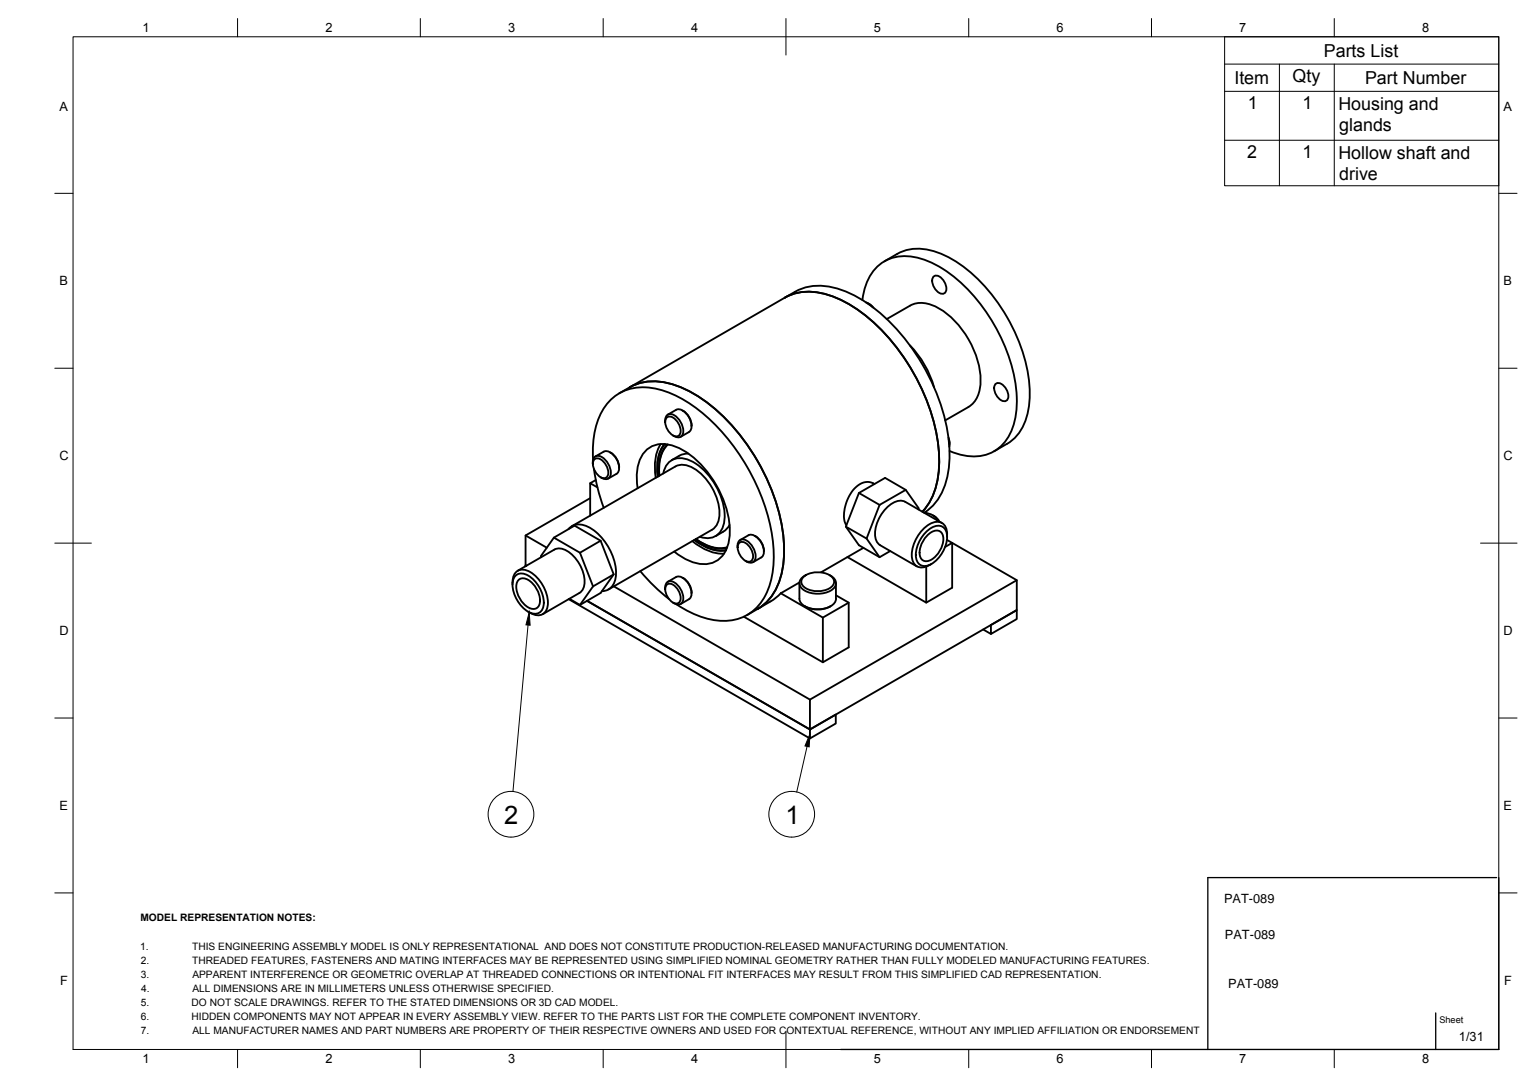
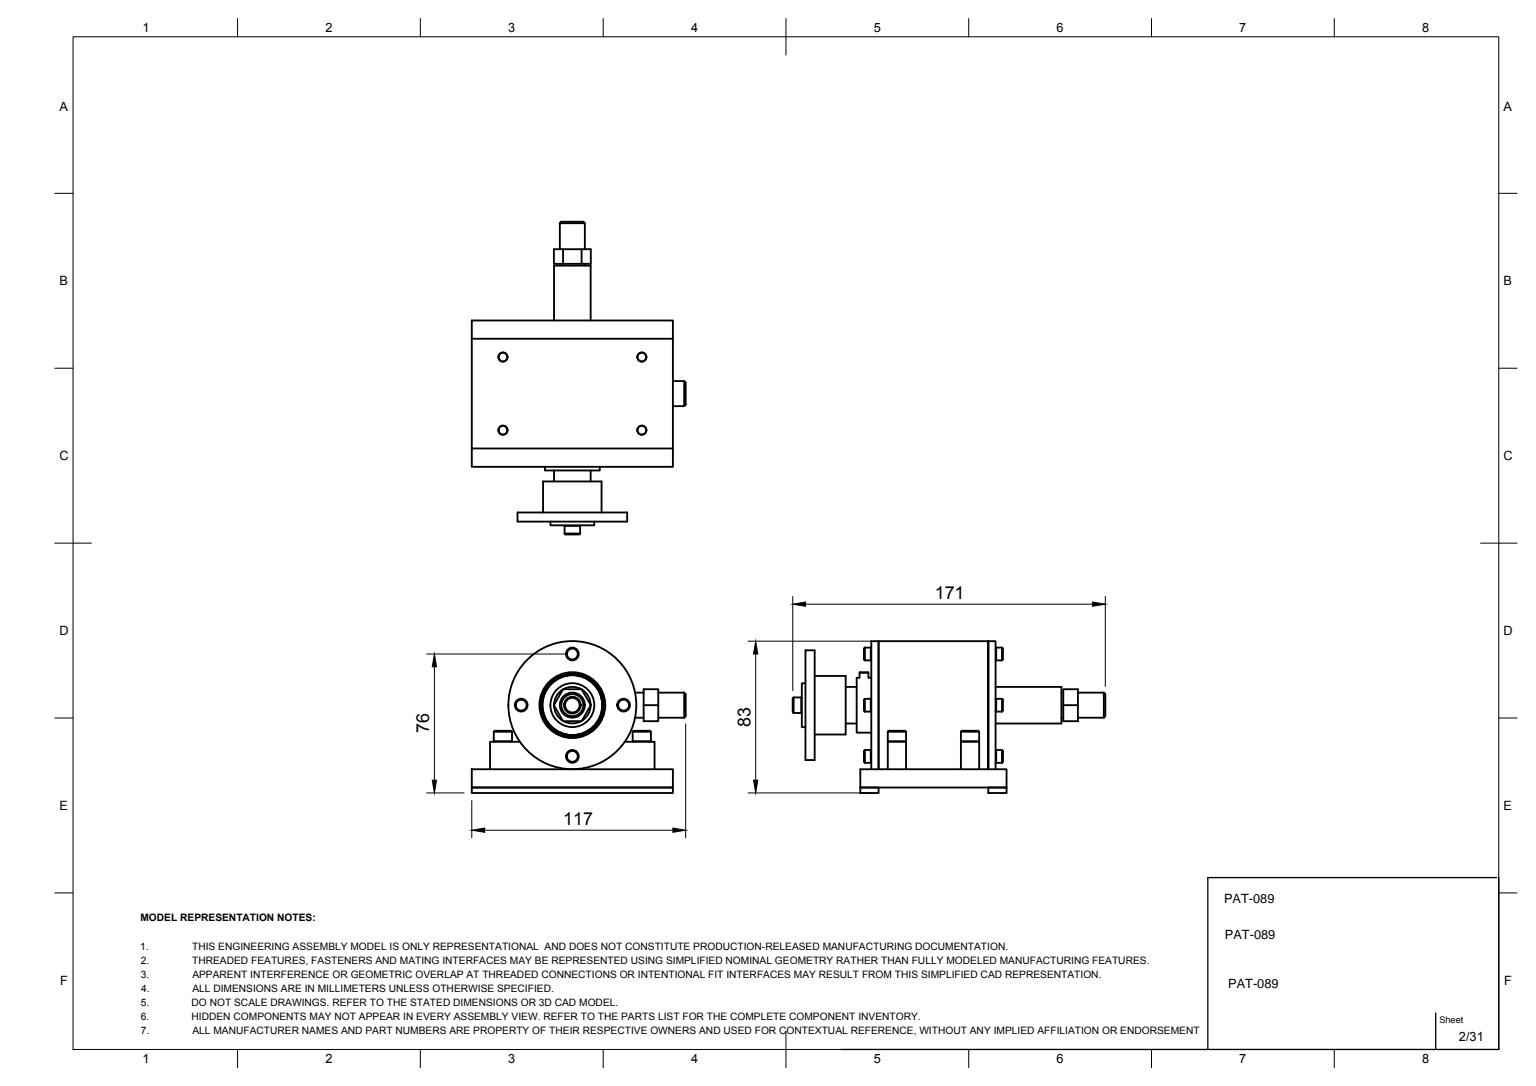
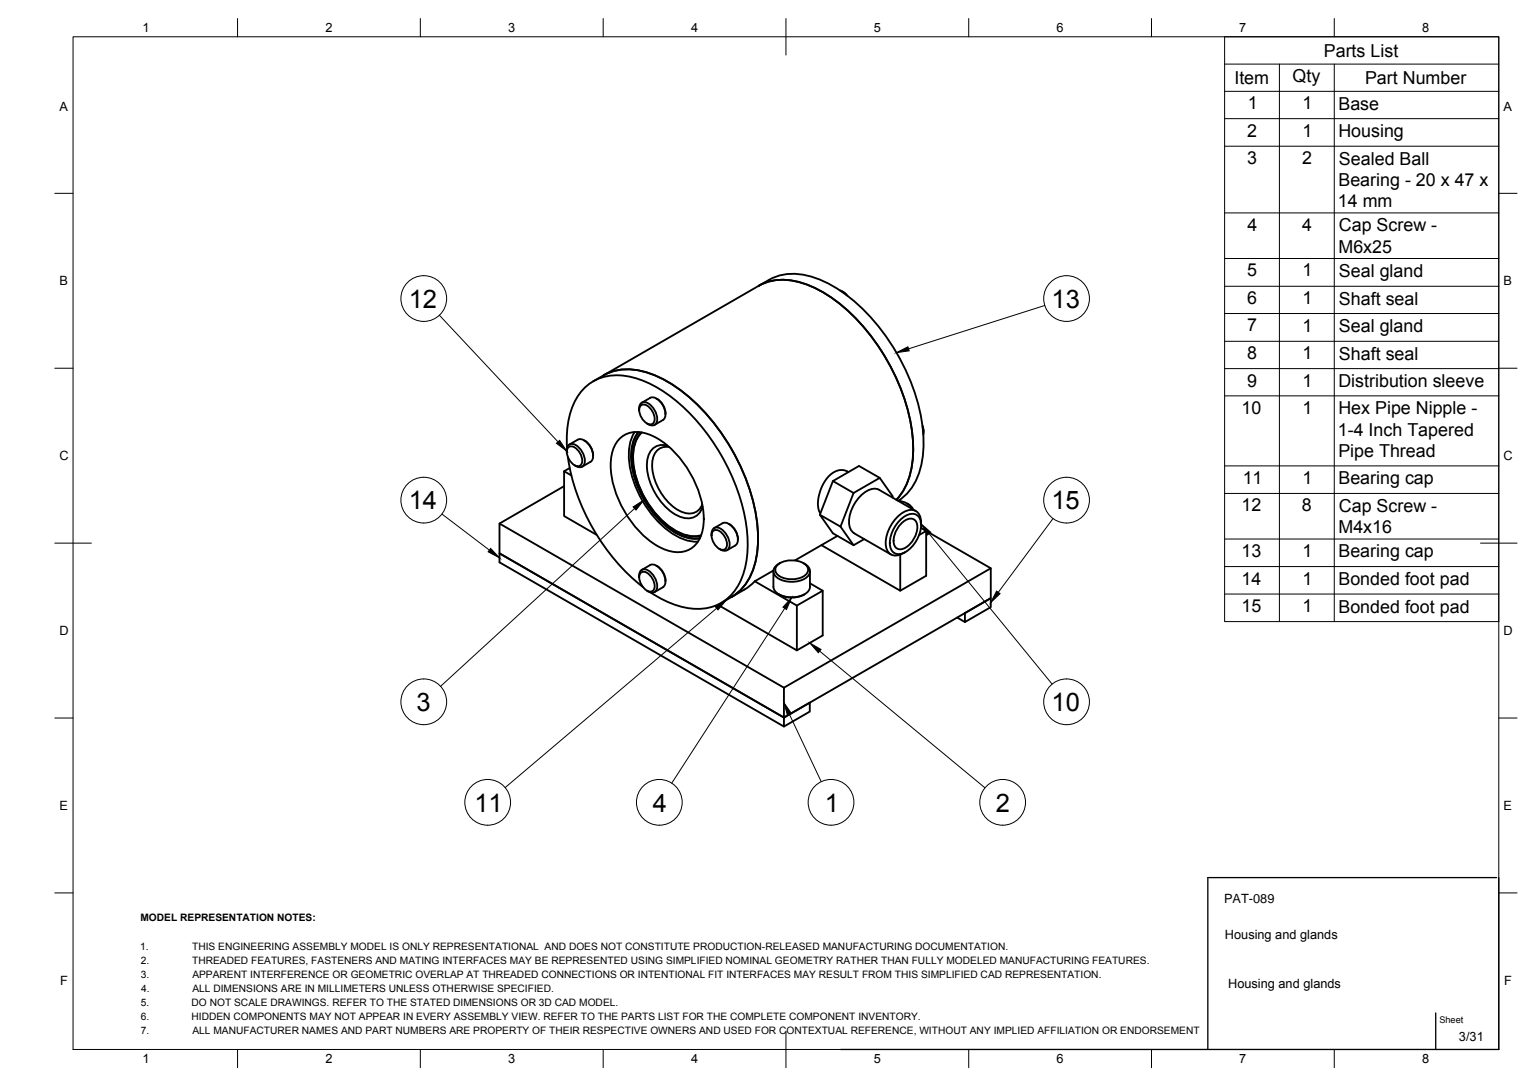
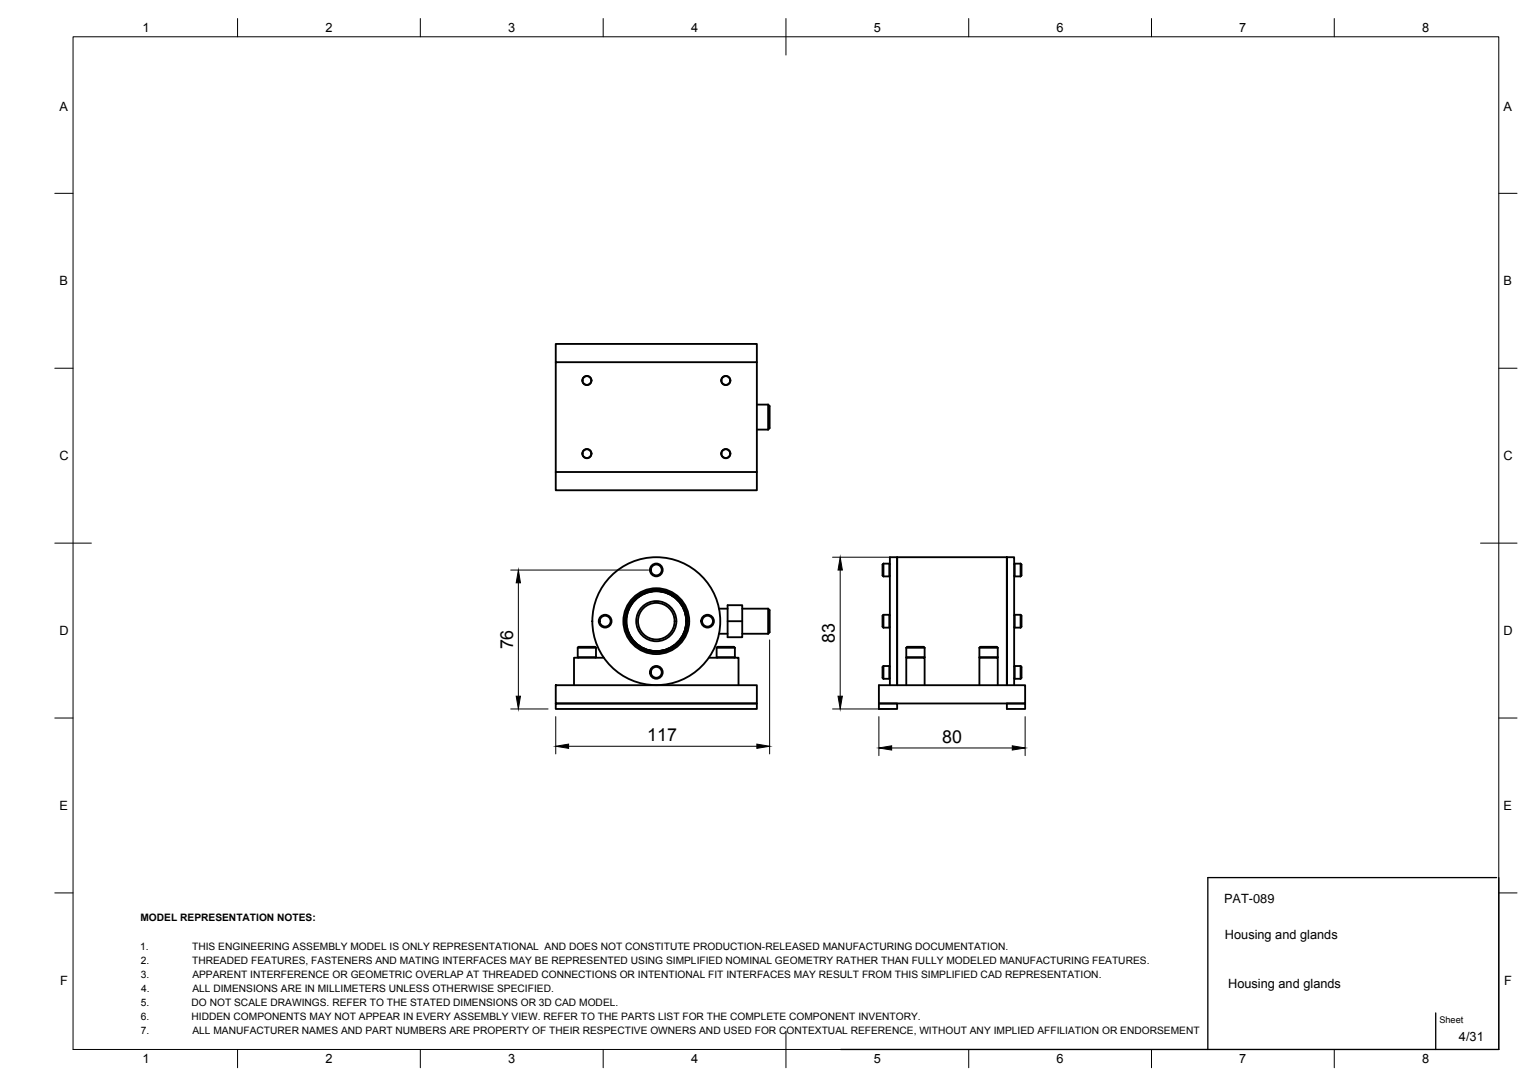
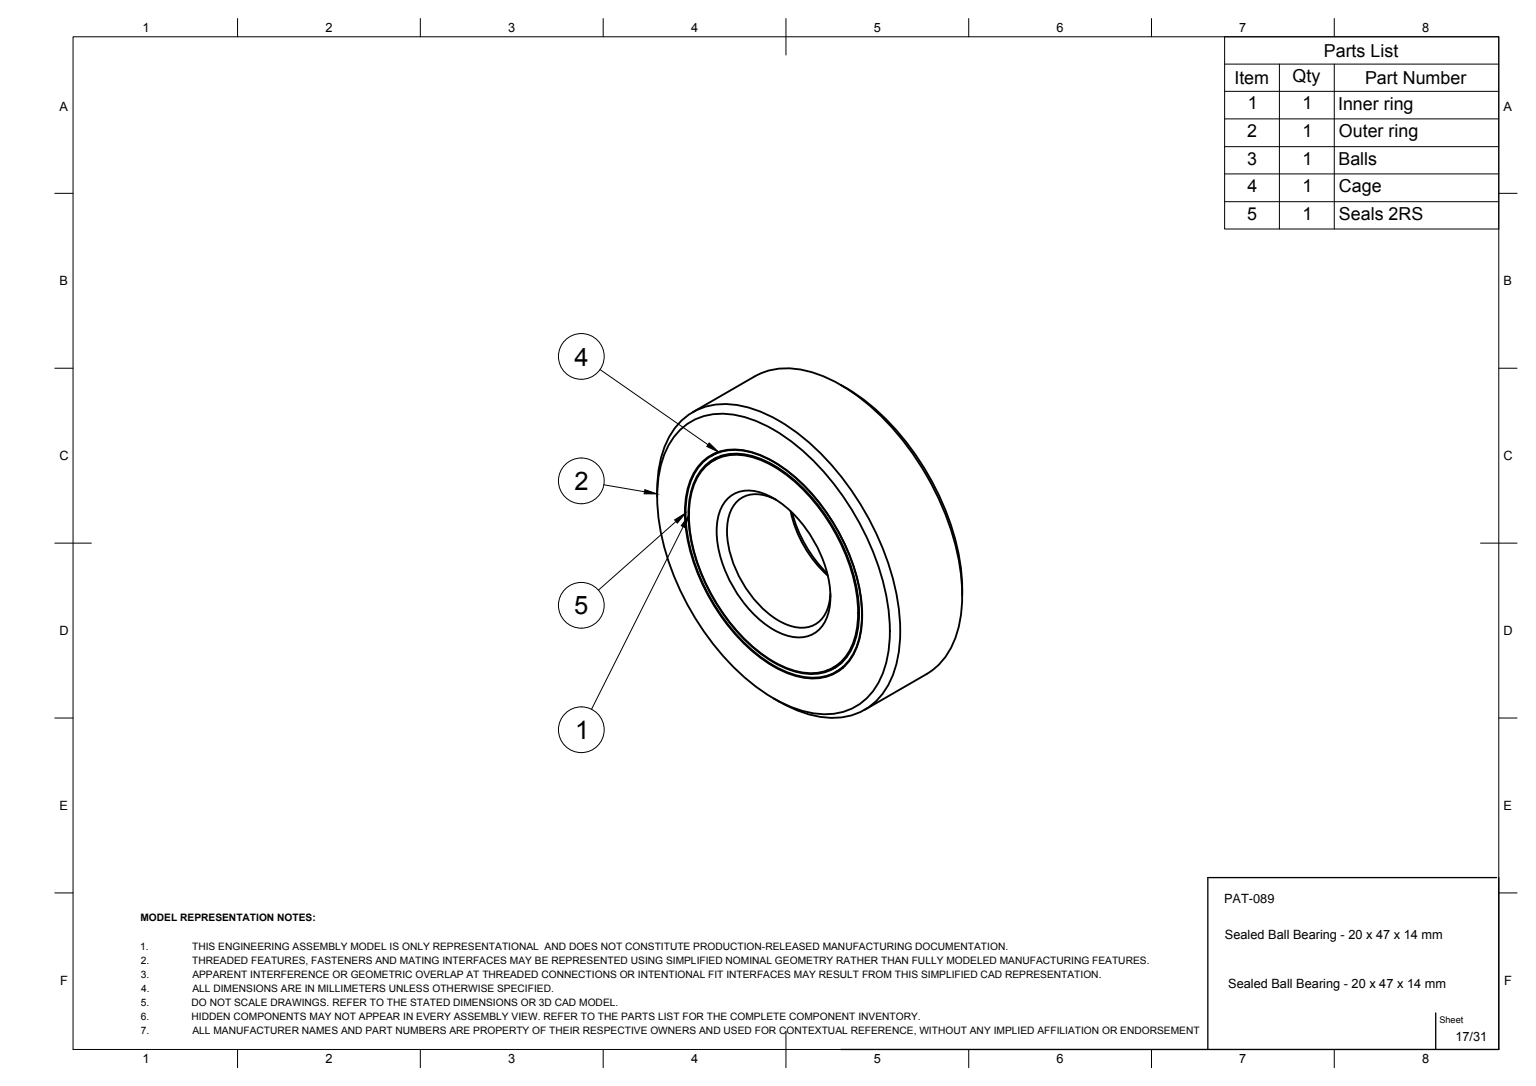
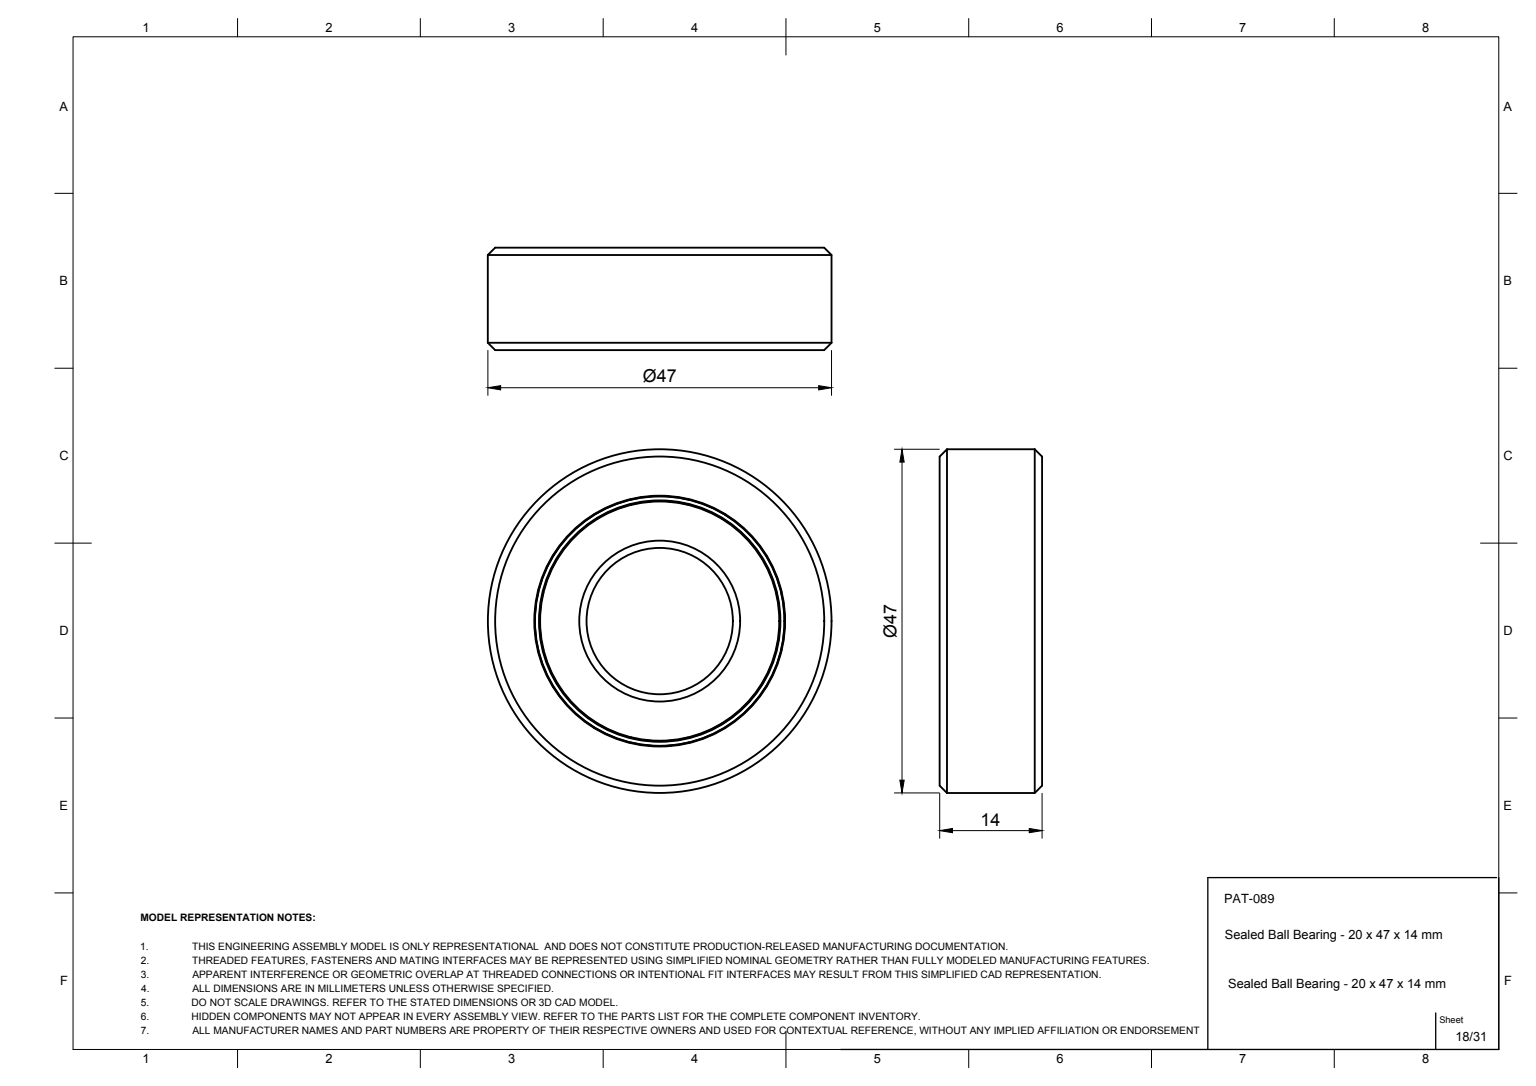
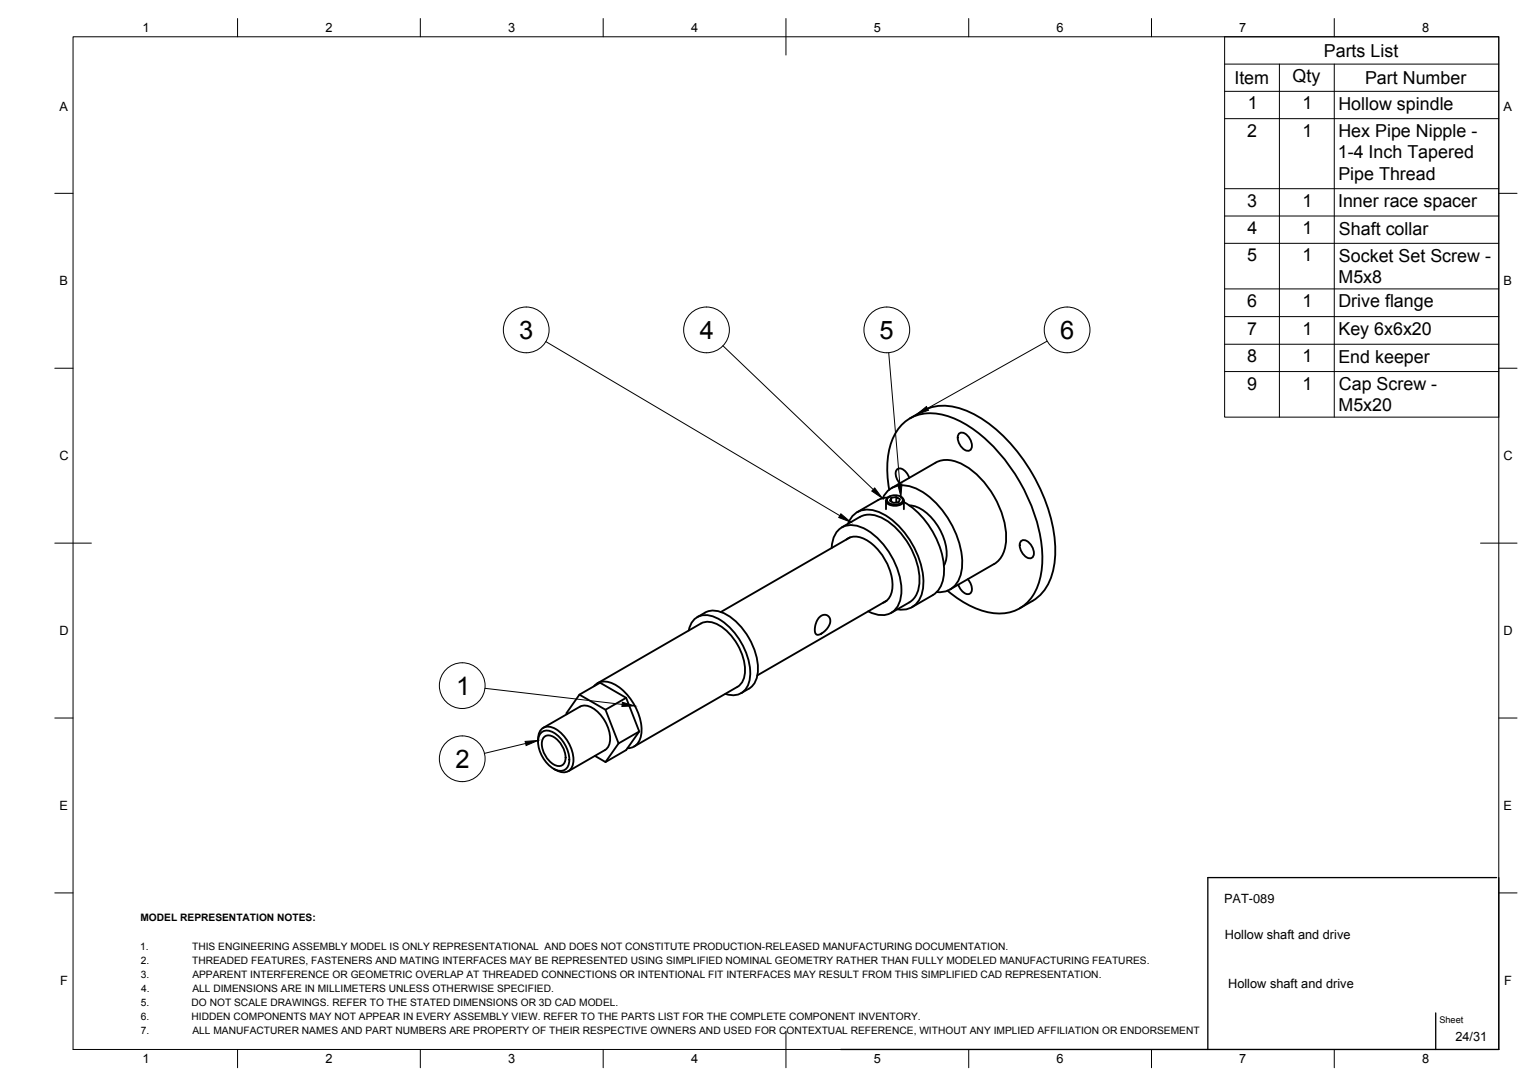
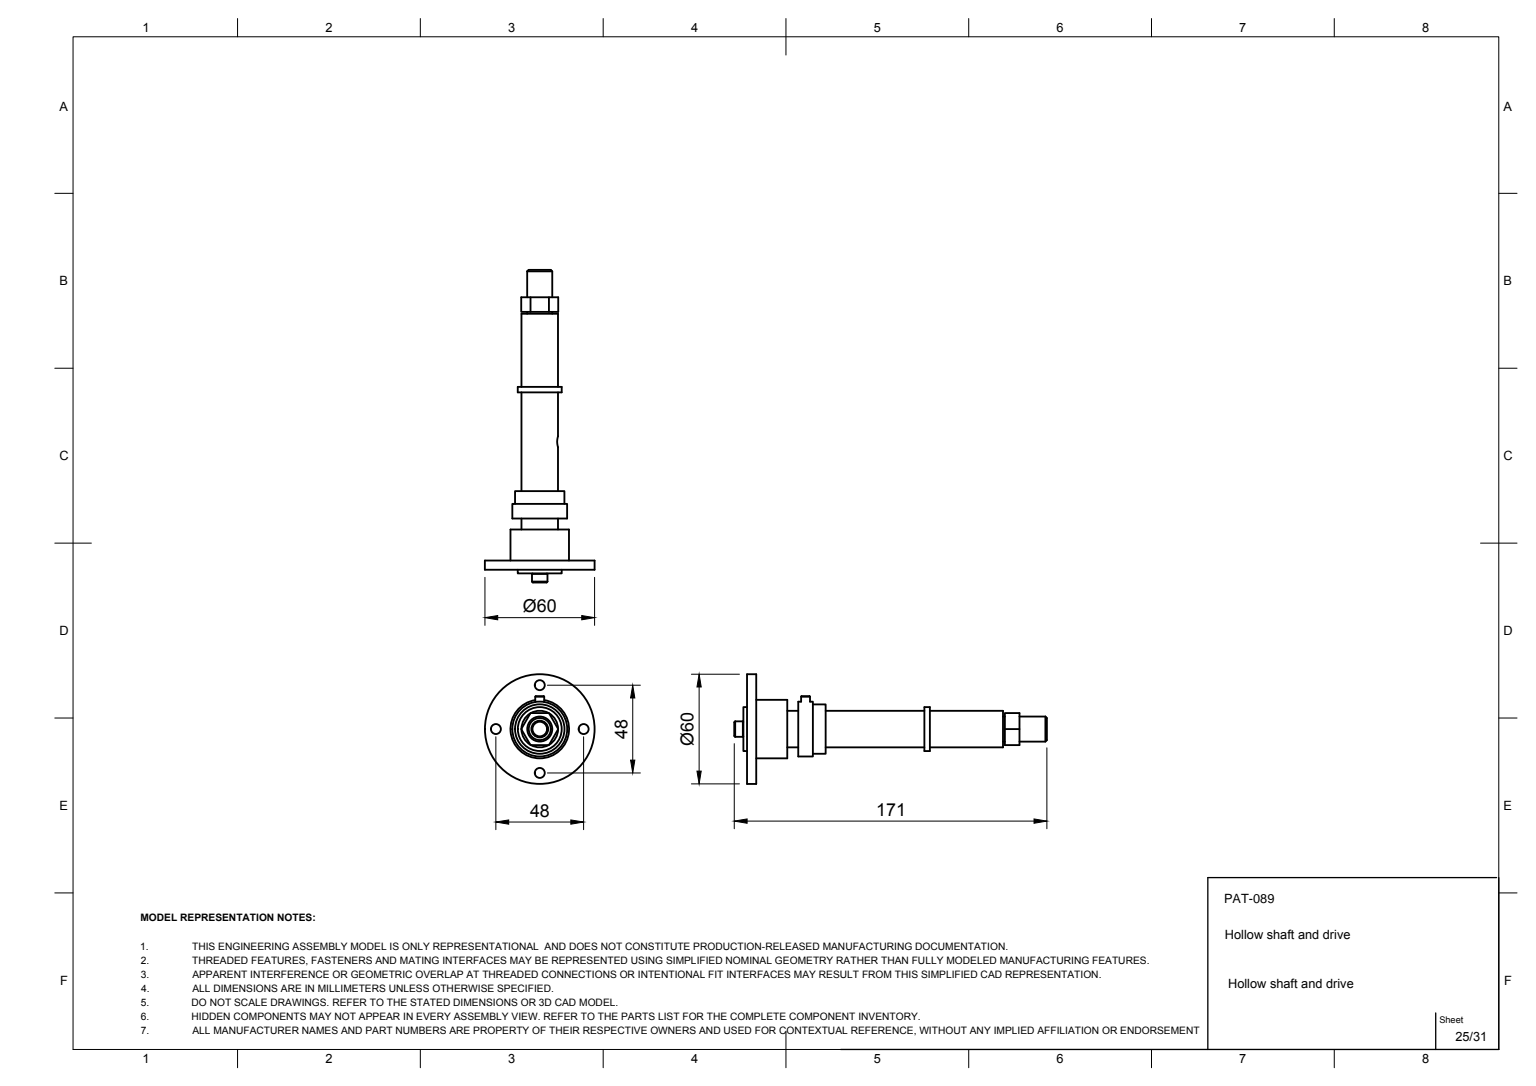
ISO-10303-21;
HEADER;
/* Generated by software containing ST-Developer
 * from STEP Tools, Inc. (www.steptools.com) 
 */

FILE_DESCRIPTION(
/* description */ ('Rotary union on bearing shaft'),
/* implementation_level */ '2;1');

FILE_NAME(
/* name */ 'PAT-089',
/* time_stamp */ '2026-10-28T03:24:01-07:00',
/* author */ (''),
/* organization */ (''),
/* preprocessor_version */ 'ST-DEVELOPER v20.2',
/* originating_system */ 'Autodesk Translation Framework v15.17.0.0',
/* authorisation */ '');

FILE_SCHEMA (('AUTOMOTIVE_DESIGN { 1 0 10303 214 3 1 1 }'));
ENDSEC;

DATA;
#10=MECHANICAL_DESIGN_GEOMETRIC_PRESENTATION_REPRESENTATION('',(#313,#314,
#315,#316,#317,#318,#319,#320,#321,#322,#323,#324,#325,#326,#327,#328,#329,
#330,#331,#332,#333,#334,#335,#336,#337,#338,#339,#340,#341,#342,#343,#344,
#345,#346,#347),#9448);
#11=ORIENTED_CLOSED_SHELL('',*,#4893,.F.);
#12=ORIENTED_CLOSED_SHELL('',*,#4895,.F.);
#13=ORIENTED_CLOSED_SHELL('',*,#4905,.F.);
#14=BREP_WITH_VOIDS('Body1',#4892,(#11));
#15=BREP_WITH_VOIDS('Body1',#4894,(#12));
#16=BREP_WITH_VOIDS('Body1',#4904,(#13));
#17=ITEM_DEFINED_TRANSFORMATION($,$,#5428,#5556);
#18=ITEM_DEFINED_TRANSFORMATION($,$,#5448,#5557);
#19=ITEM_DEFINED_TRANSFORMATION($,$,#5468,#5558);
#20=ITEM_DEFINED_TRANSFORMATION($,$,#5485,#5559);
#21=ITEM_DEFINED_TRANSFORMATION($,$,#5539,#5560);
#22=ITEM_DEFINED_TRANSFORMATION($,$,#5206,#5737);
#23=ITEM_DEFINED_TRANSFORMATION($,$,#5225,#5738);
#24=ITEM_DEFINED_TRANSFORMATION($,$,#5305,#5739);
#25=ITEM_DEFINED_TRANSFORMATION($,$,#5322,#5740);
#26=ITEM_DEFINED_TRANSFORMATION($,$,#5326,#5741);
#27=ITEM_DEFINED_TRANSFORMATION($,$,#5343,#5742);
#28=ITEM_DEFINED_TRANSFORMATION($,$,#5347,#5743);
#29=ITEM_DEFINED_TRANSFORMATION($,$,#5363,#5744);
#30=ITEM_DEFINED_TRANSFORMATION($,$,#5388,#5745);
#31=ITEM_DEFINED_TRANSFORMATION($,$,#5413,#5746);
#32=ITEM_DEFINED_TRANSFORMATION($,$,#5420,#5747);
#33=ITEM_DEFINED_TRANSFORMATION($,$,#5427,#5748);
#34=ITEM_DEFINED_TRANSFORMATION($,$,#5561,#5749);
#35=ITEM_DEFINED_TRANSFORMATION($,$,#5561,#5750);
#36=ITEM_DEFINED_TRANSFORMATION($,$,#5427,#5751);
#37=ITEM_DEFINED_TRANSFORMATION($,$,#5561,#5752);
#38=ITEM_DEFINED_TRANSFORMATION($,$,#5561,#5753);
#39=ITEM_DEFINED_TRANSFORMATION($,$,#5713,#5754);
#40=ITEM_DEFINED_TRANSFORMATION($,$,#5587,#5755);
#41=ITEM_DEFINED_TRANSFORMATION($,$,#5587,#5756);
#42=ITEM_DEFINED_TRANSFORMATION($,$,#5587,#5757);
#43=ITEM_DEFINED_TRANSFORMATION($,$,#5587,#5758);
#44=ITEM_DEFINED_TRANSFORMATION($,$,#5587,#5759);
#45=ITEM_DEFINED_TRANSFORMATION($,$,#5587,#5760);
#46=ITEM_DEFINED_TRANSFORMATION($,$,#5587,#5761);
#47=ITEM_DEFINED_TRANSFORMATION($,$,#5587,#5762);
#48=ITEM_DEFINED_TRANSFORMATION($,$,#5614,#5817);
#49=ITEM_DEFINED_TRANSFORMATION($,$,#5652,#5818);
#50=ITEM_DEFINED_TRANSFORMATION($,$,#5661,#5819);
#51=ITEM_DEFINED_TRANSFORMATION($,$,#5676,#5820);
#52=ITEM_DEFINED_TRANSFORMATION($,$,#5704,#5821);
#53=ITEM_DEFINED_TRANSFORMATION($,$,#5713,#5822);
#54=ITEM_DEFINED_TRANSFORMATION($,$,#5763,#5823);
#55=ITEM_DEFINED_TRANSFORMATION($,$,#5780,#5824);
#56=ITEM_DEFINED_TRANSFORMATION($,$,#5791,#5825);
#57=ITEM_DEFINED_TRANSFORMATION($,$,#5205,#5826);
#58=ITEM_DEFINED_TRANSFORMATION($,$,#5613,#5827);
#59=(
REPRESENTATION_RELATIONSHIP($,$,#9571,#9570)
REPRESENTATION_RELATIONSHIP_WITH_TRANSFORMATION(#17)
SHAPE_REPRESENTATION_RELATIONSHIP()
);
#60=(
REPRESENTATION_RELATIONSHIP($,$,#9572,#9570)
REPRESENTATION_RELATIONSHIP_WITH_TRANSFORMATION(#18)
SHAPE_REPRESENTATION_RELATIONSHIP()
);
#61=(
REPRESENTATION_RELATIONSHIP($,$,#9573,#9570)
REPRESENTATION_RELATIONSHIP_WITH_TRANSFORMATION(#19)
SHAPE_REPRESENTATION_RELATIONSHIP()
);
#62=(
REPRESENTATION_RELATIONSHIP($,$,#9574,#9570)
REPRESENTATION_RELATIONSHIP_WITH_TRANSFORMATION(#20)
SHAPE_REPRESENTATION_RELATIONSHIP()
);
#63=(
REPRESENTATION_RELATIONSHIP($,$,#9575,#9570)
REPRESENTATION_RELATIONSHIP_WITH_TRANSFORMATION(#21)
SHAPE_REPRESENTATION_RELATIONSHIP()
);
#64=(
REPRESENTATION_RELATIONSHIP($,$,#9559,#9558)
REPRESENTATION_RELATIONSHIP_WITH_TRANSFORMATION(#22)
SHAPE_REPRESENTATION_RELATIONSHIP()
);
#65=(
REPRESENTATION_RELATIONSHIP($,$,#9560,#9558)
REPRESENTATION_RELATIONSHIP_WITH_TRANSFORMATION(#23)
SHAPE_REPRESENTATION_RELATIONSHIP()
);
#66=(
REPRESENTATION_RELATIONSHIP($,$,#9561,#9558)
REPRESENTATION_RELATIONSHIP_WITH_TRANSFORMATION(#24)
SHAPE_REPRESENTATION_RELATIONSHIP()
);
#67=(
REPRESENTATION_RELATIONSHIP($,$,#9562,#9558)
REPRESENTATION_RELATIONSHIP_WITH_TRANSFORMATION(#25)
SHAPE_REPRESENTATION_RELATIONSHIP()
);
#68=(
REPRESENTATION_RELATIONSHIP($,$,#9563,#9558)
REPRESENTATION_RELATIONSHIP_WITH_TRANSFORMATION(#26)
SHAPE_REPRESENTATION_RELATIONSHIP()
);
#69=(
REPRESENTATION_RELATIONSHIP($,$,#9564,#9558)
REPRESENTATION_RELATIONSHIP_WITH_TRANSFORMATION(#27)
SHAPE_REPRESENTATION_RELATIONSHIP()
);
#70=(
REPRESENTATION_RELATIONSHIP($,$,#9565,#9558)
REPRESENTATION_RELATIONSHIP_WITH_TRANSFORMATION(#28)
SHAPE_REPRESENTATION_RELATIONSHIP()
);
#71=(
REPRESENTATION_RELATIONSHIP($,$,#9566,#9558)
REPRESENTATION_RELATIONSHIP_WITH_TRANSFORMATION(#29)
SHAPE_REPRESENTATION_RELATIONSHIP()
);
#72=(
REPRESENTATION_RELATIONSHIP($,$,#9567,#9558)
REPRESENTATION_RELATIONSHIP_WITH_TRANSFORMATION(#30)
SHAPE_REPRESENTATION_RELATIONSHIP()
);
#73=(
REPRESENTATION_RELATIONSHIP($,$,#9568,#9558)
REPRESENTATION_RELATIONSHIP_WITH_TRANSFORMATION(#31)
SHAPE_REPRESENTATION_RELATIONSHIP()
);
#74=(
REPRESENTATION_RELATIONSHIP($,$,#9569,#9558)
REPRESENTATION_RELATIONSHIP_WITH_TRANSFORMATION(#32)
SHAPE_REPRESENTATION_RELATIONSHIP()
);
#75=(
REPRESENTATION_RELATIONSHIP($,$,#9570,#9558)
REPRESENTATION_RELATIONSHIP_WITH_TRANSFORMATION(#33)
SHAPE_REPRESENTATION_RELATIONSHIP()
);
#76=(
REPRESENTATION_RELATIONSHIP($,$,#9576,#9558)
REPRESENTATION_RELATIONSHIP_WITH_TRANSFORMATION(#34)
SHAPE_REPRESENTATION_RELATIONSHIP()
);
#77=(
REPRESENTATION_RELATIONSHIP($,$,#9576,#9558)
REPRESENTATION_RELATIONSHIP_WITH_TRANSFORMATION(#35)
SHAPE_REPRESENTATION_RELATIONSHIP()
);
#78=(
REPRESENTATION_RELATIONSHIP($,$,#9570,#9558)
REPRESENTATION_RELATIONSHIP_WITH_TRANSFORMATION(#36)
SHAPE_REPRESENTATION_RELATIONSHIP()
);
#79=(
REPRESENTATION_RELATIONSHIP($,$,#9576,#9558)
REPRESENTATION_RELATIONSHIP_WITH_TRANSFORMATION(#37)
SHAPE_REPRESENTATION_RELATIONSHIP()
);
#80=(
REPRESENTATION_RELATIONSHIP($,$,#9576,#9558)
REPRESENTATION_RELATIONSHIP_WITH_TRANSFORMATION(#38)
SHAPE_REPRESENTATION_RELATIONSHIP()
);
#81=(
REPRESENTATION_RELATIONSHIP($,$,#9584,#9558)
REPRESENTATION_RELATIONSHIP_WITH_TRANSFORMATION(#39)
SHAPE_REPRESENTATION_RELATIONSHIP()
);
#82=(
REPRESENTATION_RELATIONSHIP($,$,#9577,#9558)
REPRESENTATION_RELATIONSHIP_WITH_TRANSFORMATION(#40)
SHAPE_REPRESENTATION_RELATIONSHIP()
);
#83=(
REPRESENTATION_RELATIONSHIP($,$,#9577,#9558)
REPRESENTATION_RELATIONSHIP_WITH_TRANSFORMATION(#41)
SHAPE_REPRESENTATION_RELATIONSHIP()
);
#84=(
REPRESENTATION_RELATIONSHIP($,$,#9577,#9558)
REPRESENTATION_RELATIONSHIP_WITH_TRANSFORMATION(#42)
SHAPE_REPRESENTATION_RELATIONSHIP()
);
#85=(
REPRESENTATION_RELATIONSHIP($,$,#9577,#9558)
REPRESENTATION_RELATIONSHIP_WITH_TRANSFORMATION(#43)
SHAPE_REPRESENTATION_RELATIONSHIP()
);
#86=(
REPRESENTATION_RELATIONSHIP($,$,#9577,#9558)
REPRESENTATION_RELATIONSHIP_WITH_TRANSFORMATION(#44)
SHAPE_REPRESENTATION_RELATIONSHIP()
);
#87=(
REPRESENTATION_RELATIONSHIP($,$,#9577,#9558)
REPRESENTATION_RELATIONSHIP_WITH_TRANSFORMATION(#45)
SHAPE_REPRESENTATION_RELATIONSHIP()
);
#88=(
REPRESENTATION_RELATIONSHIP($,$,#9577,#9558)
REPRESENTATION_RELATIONSHIP_WITH_TRANSFORMATION(#46)
SHAPE_REPRESENTATION_RELATIONSHIP()
);
#89=(
REPRESENTATION_RELATIONSHIP($,$,#9577,#9558)
REPRESENTATION_RELATIONSHIP_WITH_TRANSFORMATION(#47)
SHAPE_REPRESENTATION_RELATIONSHIP()
);
#90=(
REPRESENTATION_RELATIONSHIP($,$,#9579,#9578)
REPRESENTATION_RELATIONSHIP_WITH_TRANSFORMATION(#48)
SHAPE_REPRESENTATION_RELATIONSHIP()
);
#91=(
REPRESENTATION_RELATIONSHIP($,$,#9580,#9578)
REPRESENTATION_RELATIONSHIP_WITH_TRANSFORMATION(#49)
SHAPE_REPRESENTATION_RELATIONSHIP()
);
#92=(
REPRESENTATION_RELATIONSHIP($,$,#9581,#9578)
REPRESENTATION_RELATIONSHIP_WITH_TRANSFORMATION(#50)
SHAPE_REPRESENTATION_RELATIONSHIP()
);
#93=(
REPRESENTATION_RELATIONSHIP($,$,#9582,#9578)
REPRESENTATION_RELATIONSHIP_WITH_TRANSFORMATION(#51)
SHAPE_REPRESENTATION_RELATIONSHIP()
);
#94=(
REPRESENTATION_RELATIONSHIP($,$,#9583,#9578)
REPRESENTATION_RELATIONSHIP_WITH_TRANSFORMATION(#52)
SHAPE_REPRESENTATION_RELATIONSHIP()
);
#95=(
REPRESENTATION_RELATIONSHIP($,$,#9584,#9578)
REPRESENTATION_RELATIONSHIP_WITH_TRANSFORMATION(#53)
SHAPE_REPRESENTATION_RELATIONSHIP()
);
#96=(
REPRESENTATION_RELATIONSHIP($,$,#9585,#9578)
REPRESENTATION_RELATIONSHIP_WITH_TRANSFORMATION(#54)
SHAPE_REPRESENTATION_RELATIONSHIP()
);
#97=(
REPRESENTATION_RELATIONSHIP($,$,#9586,#9578)
REPRESENTATION_RELATIONSHIP_WITH_TRANSFORMATION(#55)
SHAPE_REPRESENTATION_RELATIONSHIP()
);
#98=(
REPRESENTATION_RELATIONSHIP($,$,#9587,#9578)
REPRESENTATION_RELATIONSHIP_WITH_TRANSFORMATION(#56)
SHAPE_REPRESENTATION_RELATIONSHIP()
);
#99=(
REPRESENTATION_RELATIONSHIP($,$,#9558,#9557)
REPRESENTATION_RELATIONSHIP_WITH_TRANSFORMATION(#57)
SHAPE_REPRESENTATION_RELATIONSHIP()
);
#100=(
REPRESENTATION_RELATIONSHIP($,$,#9578,#9557)
REPRESENTATION_RELATIONSHIP_WITH_TRANSFORMATION(#58)
SHAPE_REPRESENTATION_RELATIONSHIP()
);
#101=CONTEXT_DEPENDENT_SHAPE_REPRESENTATION(#59,#9503);
#102=CONTEXT_DEPENDENT_SHAPE_REPRESENTATION(#60,#9504);
#103=CONTEXT_DEPENDENT_SHAPE_REPRESENTATION(#61,#9505);
#104=CONTEXT_DEPENDENT_SHAPE_REPRESENTATION(#62,#9506);
#105=CONTEXT_DEPENDENT_SHAPE_REPRESENTATION(#63,#9507);
#106=CONTEXT_DEPENDENT_SHAPE_REPRESENTATION(#64,#9517);
#107=CONTEXT_DEPENDENT_SHAPE_REPRESENTATION(#65,#9518);
#108=CONTEXT_DEPENDENT_SHAPE_REPRESENTATION(#66,#9519);
#109=CONTEXT_DEPENDENT_SHAPE_REPRESENTATION(#67,#9520);
#110=CONTEXT_DEPENDENT_SHAPE_REPRESENTATION(#68,#9521);
#111=CONTEXT_DEPENDENT_SHAPE_REPRESENTATION(#69,#9522);
#112=CONTEXT_DEPENDENT_SHAPE_REPRESENTATION(#70,#9523);
#113=CONTEXT_DEPENDENT_SHAPE_REPRESENTATION(#71,#9524);
#114=CONTEXT_DEPENDENT_SHAPE_REPRESENTATION(#72,#9525);
#115=CONTEXT_DEPENDENT_SHAPE_REPRESENTATION(#73,#9526);
#116=CONTEXT_DEPENDENT_SHAPE_REPRESENTATION(#74,#9527);
#117=CONTEXT_DEPENDENT_SHAPE_REPRESENTATION(#75,#9528);
#118=CONTEXT_DEPENDENT_SHAPE_REPRESENTATION(#76,#9529);
#119=CONTEXT_DEPENDENT_SHAPE_REPRESENTATION(#77,#9530);
#120=CONTEXT_DEPENDENT_SHAPE_REPRESENTATION(#78,#9531);
#121=CONTEXT_DEPENDENT_SHAPE_REPRESENTATION(#79,#9532);
#122=CONTEXT_DEPENDENT_SHAPE_REPRESENTATION(#80,#9533);
#123=CONTEXT_DEPENDENT_SHAPE_REPRESENTATION(#81,#9534);
#124=CONTEXT_DEPENDENT_SHAPE_REPRESENTATION(#82,#9535);
#125=CONTEXT_DEPENDENT_SHAPE_REPRESENTATION(#83,#9536);
#126=CONTEXT_DEPENDENT_SHAPE_REPRESENTATION(#84,#9537);
#127=CONTEXT_DEPENDENT_SHAPE_REPRESENTATION(#85,#9538);
#128=CONTEXT_DEPENDENT_SHAPE_REPRESENTATION(#86,#9539);
#129=CONTEXT_DEPENDENT_SHAPE_REPRESENTATION(#87,#9540);
#130=CONTEXT_DEPENDENT_SHAPE_REPRESENTATION(#88,#9541);
#131=CONTEXT_DEPENDENT_SHAPE_REPRESENTATION(#89,#9542);
#132=CONTEXT_DEPENDENT_SHAPE_REPRESENTATION(#90,#9546);
#133=CONTEXT_DEPENDENT_SHAPE_REPRESENTATION(#91,#9547);
#134=CONTEXT_DEPENDENT_SHAPE_REPRESENTATION(#92,#9548);
#135=CONTEXT_DEPENDENT_SHAPE_REPRESENTATION(#93,#9549);
#136=CONTEXT_DEPENDENT_SHAPE_REPRESENTATION(#94,#9550);
#137=CONTEXT_DEPENDENT_SHAPE_REPRESENTATION(#95,#9551);
#138=CONTEXT_DEPENDENT_SHAPE_REPRESENTATION(#96,#9552);
#139=CONTEXT_DEPENDENT_SHAPE_REPRESENTATION(#97,#9553);
#140=CONTEXT_DEPENDENT_SHAPE_REPRESENTATION(#98,#9554);
#141=CONTEXT_DEPENDENT_SHAPE_REPRESENTATION(#99,#9555);
#142=CONTEXT_DEPENDENT_SHAPE_REPRESENTATION(#100,#9556);
#143=NEXT_ASSEMBLY_USAGE_OCCURRENCE('Inner ring:1','Inner ring:1',
'Inner ring:1',#9602,#9603,'Inner ring:1');
#144=NEXT_ASSEMBLY_USAGE_OCCURRENCE('Outer ring:1','Outer ring:1',
'Outer ring:1',#9602,#9604,'Outer ring:1');
#145=NEXT_ASSEMBLY_USAGE_OCCURRENCE('Balls:1','Balls:1','Balls:1',#9602,
#9605,'Balls:1');
#146=NEXT_ASSEMBLY_USAGE_OCCURRENCE('Cage:1','Cage:1','Cage:1',#9602,#9606,
'Cage:1');
#147=NEXT_ASSEMBLY_USAGE_OCCURRENCE('Seals 2RS:1','Seals 2RS:1',
'Seals 2RS:1',#9602,#9607,'Seals 2RS:1');
#148=NEXT_ASSEMBLY_USAGE_OCCURRENCE('Base:1','Base:1','Base:1',#9590,#9591,
'Base:1');
#149=NEXT_ASSEMBLY_USAGE_OCCURRENCE('Housing:1','Housing:1','Housing:1',
#9590,#9592,'Housing:1');
#150=NEXT_ASSEMBLY_USAGE_OCCURRENCE('Seal gland:1','Seal gland:1',
'Seal gland:1',#9590,#9593,'Seal gland:1');
#151=NEXT_ASSEMBLY_USAGE_OCCURRENCE('Shaft seal:1','Shaft seal:1',
'Shaft seal:1',#9590,#9594,'Shaft seal:1');
#152=NEXT_ASSEMBLY_USAGE_OCCURRENCE('Seal gland (1):1',
'Seal gland (1):1','Seal gland (1):1',#9590,#9595,'Seal gland (1):1');
#153=NEXT_ASSEMBLY_USAGE_OCCURRENCE('Shaft seal (1):1',
'Shaft seal (1):1','Shaft seal (1):1',#9590,#9596,'Shaft seal (1):1');
#154=NEXT_ASSEMBLY_USAGE_OCCURRENCE('Distribution sleeve:1',
'Distribution sleeve:1','Distribution sleeve:1',#9590,#9597,
'Distribution sleeve:1');
#155=NEXT_ASSEMBLY_USAGE_OCCURRENCE('Bearing cap:1','Bearing cap:1',
'Bearing cap:1',#9590,#9598,'Bearing cap:1');
#156=NEXT_ASSEMBLY_USAGE_OCCURRENCE('Bearing cap (1):1',
'Bearing cap (1):1','Bearing cap (1):1',#9590,#9599,'Bearing cap (1):1');
#157=NEXT_ASSEMBLY_USAGE_OCCURRENCE('Bonded foot pad:1',
'Bonded foot pad:1','Bonded foot pad:1',#9590,#9600,'Bonded foot pad:1');
#158=NEXT_ASSEMBLY_USAGE_OCCURRENCE('Bonded foot pad (1):1',
'Bonded foot pad (1):1','Bonded foot pad (1):1',#9590,#9601,
'Bonded foot pad (1):1');
#159=NEXT_ASSEMBLY_USAGE_OCCURRENCE(
'Sealed Ball Bearing - 20 x 47 x 14 mm:2',
'Sealed Ball Bearing - 20 x 47 x 14 mm:2',
'Sealed Ball Bearing - 20 x 47 x 14 mm:2',#9590,#9602,
'Sealed Ball Bearing - 20 x 47 x 14 mm:2');
#160=NEXT_ASSEMBLY_USAGE_OCCURRENCE('Cap Screw - M6x25:2',
'Cap Screw - M6x25:2','Cap Screw - M6x25:2',#9590,#9608,
'Cap Screw - M6x25:2');
#161=NEXT_ASSEMBLY_USAGE_OCCURRENCE('Cap Screw - M6x25:3',
'Cap Screw - M6x25:3','Cap Screw - M6x25:3',#9590,#9608,
'Cap Screw - M6x25:3');
#162=NEXT_ASSEMBLY_USAGE_OCCURRENCE(
'Sealed Ball Bearing - 20 x 47 x 14 mm:3',
'Sealed Ball Bearing - 20 x 47 x 14 mm:3',
'Sealed Ball Bearing - 20 x 47 x 14 mm:3',#9590,#9602,
'Sealed Ball Bearing - 20 x 47 x 14 mm:3');
#163=NEXT_ASSEMBLY_USAGE_OCCURRENCE('Cap Screw - M6x25:4',
'Cap Screw - M6x25:4','Cap Screw - M6x25:4',#9590,#9608,
'Cap Screw - M6x25:4');
#164=NEXT_ASSEMBLY_USAGE_OCCURRENCE('Cap Screw - M6x25:5',
'Cap Screw - M6x25:5','Cap Screw - M6x25:5',#9590,#9608,
'Cap Screw - M6x25:5');
#165=NEXT_ASSEMBLY_USAGE_OCCURRENCE(
'Hex Pipe Nipple - 1-4 Inch Tapered Pipe Thread:2',
'Hex Pipe Nipple - 1-4 Inch Tapered Pipe Thread:2',
'Hex Pipe Nipple - 1-4 Inch Tapered Pipe Thread:2',#9590,#9616,
'Hex Pipe Nipple - 1-4 Inch Tapered Pipe Thread:2');
#166=NEXT_ASSEMBLY_USAGE_OCCURRENCE('Cap Screw - M4x16:2',
'Cap Screw - M4x16:2','Cap Screw - M4x16:2',#9590,#9609,
'Cap Screw - M4x16:2');
#167=NEXT_ASSEMBLY_USAGE_OCCURRENCE('Cap Screw - M4x16:3',
'Cap Screw - M4x16:3','Cap Screw - M4x16:3',#9590,#9609,
'Cap Screw - M4x16:3');
#168=NEXT_ASSEMBLY_USAGE_OCCURRENCE('Cap Screw - M4x16:4',
'Cap Screw - M4x16:4','Cap Screw - M4x16:4',#9590,#9609,
'Cap Screw - M4x16:4');
#169=NEXT_ASSEMBLY_USAGE_OCCURRENCE('Cap Screw - M4x16:5',
'Cap Screw - M4x16:5','Cap Screw - M4x16:5',#9590,#9609,
'Cap Screw - M4x16:5');
#170=NEXT_ASSEMBLY_USAGE_OCCURRENCE('Cap Screw - M4x16:6',
'Cap Screw - M4x16:6','Cap Screw - M4x16:6',#9590,#9609,
'Cap Screw - M4x16:6');
#171=NEXT_ASSEMBLY_USAGE_OCCURRENCE('Cap Screw - M4x16:7',
'Cap Screw - M4x16:7','Cap Screw - M4x16:7',#9590,#9609,
'Cap Screw - M4x16:7');
#172=NEXT_ASSEMBLY_USAGE_OCCURRENCE('Cap Screw - M4x16:8',
'Cap Screw - M4x16:8','Cap Screw - M4x16:8',#9590,#9609,
'Cap Screw - M4x16:8');
#173=NEXT_ASSEMBLY_USAGE_OCCURRENCE('Cap Screw - M4x16:9',
'Cap Screw - M4x16:9','Cap Screw - M4x16:9',#9590,#9609,
'Cap Screw - M4x16:9');
#174=NEXT_ASSEMBLY_USAGE_OCCURRENCE('Hollow spindle:1',
'Hollow spindle:1','Hollow spindle:1',#9610,#9611,'Hollow spindle:1');
#175=NEXT_ASSEMBLY_USAGE_OCCURRENCE('Inner race spacer:1',
'Inner race spacer:1','Inner race spacer:1',#9610,#9612,
'Inner race spacer:1');
#176=NEXT_ASSEMBLY_USAGE_OCCURRENCE('Shaft collar:1','Shaft collar:1',
'Shaft collar:1',#9610,#9613,'Shaft collar:1');
#177=NEXT_ASSEMBLY_USAGE_OCCURRENCE('Drive flange:1','Drive flange:1',
'Drive flange:1',#9610,#9614,'Drive flange:1');
#178=NEXT_ASSEMBLY_USAGE_OCCURRENCE('End keeper:1','End keeper:1',
'End keeper:1',#9610,#9615,'End keeper:1');
#179=NEXT_ASSEMBLY_USAGE_OCCURRENCE(
'Hex Pipe Nipple - 1-4 Inch Tapered Pipe Thread:3',
'Hex Pipe Nipple - 1-4 Inch Tapered Pipe Thread:3',
'Hex Pipe Nipple - 1-4 Inch Tapered Pipe Thread:3',#9610,#9616,
'Hex Pipe Nipple - 1-4 Inch Tapered Pipe Thread:3');
#180=NEXT_ASSEMBLY_USAGE_OCCURRENCE('Socket Set Screw - M5x8:2',
'Socket Set Screw - M5x8:2','Socket Set Screw - M5x8:2',#9610,#9617,
'Socket Set Screw - M5x8:2');
#181=NEXT_ASSEMBLY_USAGE_OCCURRENCE('Key 6x6x20:2','Key 6x6x20:2',
'Key 6x6x20:2',#9610,#9618,'Key 6x6x20:2');
#182=NEXT_ASSEMBLY_USAGE_OCCURRENCE('Cap Screw - M5x20:2',
'Cap Screw - M5x20:2','Cap Screw - M5x20:2',#9610,#9619,
'Cap Screw - M5x20:2');
#183=NEXT_ASSEMBLY_USAGE_OCCURRENCE('Housing and glands:1',
'Housing and glands:1','Housing and glands:1',#9589,#9590,
'Housing and glands:1');
#184=NEXT_ASSEMBLY_USAGE_OCCURRENCE('Hollow shaft and drive:1',
'Hollow shaft and drive:1','Hollow shaft and drive:1',#9589,#9610,
'Hollow shaft and drive:1');
#185=SPHERICAL_SURFACE('',#5469,0.3969);
#186=SPHERICAL_SURFACE('',#5471,0.3969);
#187=SPHERICAL_SURFACE('',#5473,0.3969);
#188=SPHERICAL_SURFACE('',#5475,0.3969);
#189=SPHERICAL_SURFACE('',#5477,0.3969);
#190=SPHERICAL_SURFACE('',#5479,0.3969);
#191=SPHERICAL_SURFACE('',#5481,0.3969);
#192=SPHERICAL_SURFACE('',#5483,0.3969);
#193=SPHERICAL_SURFACE('',#5486,0.412776);
#194=SPHERICAL_SURFACE('',#5502,0.412776);
#195=SPHERICAL_SURFACE('',#5507,0.412776);
#196=SPHERICAL_SURFACE('',#5512,0.412776);
#197=SPHERICAL_SURFACE('',#5517,0.412776);
#198=SPHERICAL_SURFACE('',#5522,0.412776);
#199=SPHERICAL_SURFACE('',#5527,0.412776);
#200=SPHERICAL_SURFACE('',#5535,0.412776);
#201=CONICAL_SURFACE('',#5440,1.05,0.785398163397449);
#202=CONICAL_SURFACE('',#5447,1.05,0.785398163397449);
#203=CONICAL_SURFACE('',#5460,2.3,0.785398163397449);
#204=CONICAL_SURFACE('',#5464,2.3,0.785398163397449);
#205=CONICAL_SURFACE('',#5564,0.475,0.785398163397449);
#206=CONICAL_SURFACE('',#5568,0.485,0.785398163397448);
#207=CONICAL_SURFACE('',#5572,0.31,0.463647609000806);
#208=CONICAL_SURFACE('',#5576,0.27,0.785398163397448);
#209=CONICAL_SURFACE('',#5590,0.325,0.785398163397448);
#210=CONICAL_SURFACE('',#5594,0.335,0.785398163397448);
#211=CONICAL_SURFACE('',#5598,0.21,0.463647609000806);
#212=CONICAL_SURFACE('',#5602,0.18,0.785398163397448);
#213=CONICAL_SURFACE('',#5729,0.645,0.785398163397448);
#214=CONICAL_SURFACE('',#5732,0.645,0.785398163397448);
#215=CONICAL_SURFACE('',#5773,0.235,0.785398163397448);
#216=CONICAL_SURFACE('',#5777,0.2125,0.785398163397448);
#217=CONICAL_SURFACE('',#5794,0.4,0.785398163397448);
#218=CONICAL_SURFACE('',#5798,0.41,0.785398163397448);
#219=CONICAL_SURFACE('',#5802,0.26,0.463647609000806);
#220=CONICAL_SURFACE('',#5806,0.225,0.785398163397448);
#221=TOROIDAL_SURFACE('',#5323,1.075,0.075);
#222=TOROIDAL_SURFACE('',#5344,1.075,0.075);
#223=TOROIDAL_SURFACE('',#5429,1.675,0.412776);
#224=TOROIDAL_SURFACE('',#5449,1.675,0.412776);
#225=B_SPLINE_CURVE_WITH_KNOTS('',3,(#7509,#7510,#7511,#7512,#7513,#7514,
#7515,#7516,#7517,#7518,#7519,#7520,#7521,#7522,#7523,#7524,#7525,#7526),
 .UNSPECIFIED.,.F.,.F.,(4,2,2,2,2,2,2,2,4),(0.,0.259699157802782,0.519398315605563,
0.779028864963069,1.03865941432058,1.29828996367808,1.55792051303559,1.81761967083837,
2.07731882864115),.UNSPECIFIED.);
#226=B_SPLINE_CURVE_WITH_KNOTS('',3,(#7527,#7528,#7529,#7530,#7531,#7532,
#7533,#7534,#7535,#7536,#7537,#7538,#7539,#7540,#7541,#7542,#7543,#7544),
 .UNSPECIFIED.,.F.,.F.,(4,2,2,2,2,2,2,2,4),(2.07731882864115,2.33701798644393,
2.59671714424671,2.85634769360422,3.11597824296173,3.37560879231923,3.63523934167674,
3.89493849947952,4.1546376572823),.UNSPECIFIED.);
#227=B_SPLINE_CURVE_WITH_KNOTS('',3,(#7548,#7549,#7550,#7551,#7552,#7553,
#7554,#7555,#7556,#7557,#7558,#7559,#7560,#7561,#7562,#7563,#7564,#7565),
 .UNSPECIFIED.,.F.,.F.,(4,2,2,2,2,2,2,2,4),(0.,0.258756642336745,0.51751328467349,
0.776256652721243,1.035000020769,1.29374338881675,1.5524867568645,1.81124339920125,
2.07000004153799),.UNSPECIFIED.);
#228=B_SPLINE_CURVE_WITH_KNOTS('',3,(#7566,#7567,#7568,#7569,#7570,#7571,
#7572,#7573,#7574,#7575,#7576,#7577,#7578,#7579,#7580,#7581,#7582,#7583),
 .UNSPECIFIED.,.F.,.F.,(4,2,2,2,2,2,2,2,4),(2.07000004153799,2.32875668387474,
2.58751332621148,2.84625669425923,3.10500006230699,3.36374343035474,3.62248679840249,
3.88124344073924,4.14000008307598),.UNSPECIFIED.);
#229=B_SPLINE_CURVE_WITH_KNOTS('',3,(#7786,#7787,#7788,#7789,#7790,#7791,
#7792,#7793,#7794,#7795,#7796,#7797,#7798,#7799,#7800),.UNSPECIFIED.,.F.,
 .F.,(4,2,2,3,2,2,4),(-0.70773137284392,-0.519428793117576,-0.259714396558788,
0.,0.259714396558788,0.519428793117576,0.707731372984028),.UNSPECIFIED.);
#230=B_SPLINE_CURVE_WITH_KNOTS('',3,(#7812,#7813,#7814,#7815,#7816,#7817,
#7818,#7819,#7820,#7821,#7822,#7823,#7824,#7825),.UNSPECIFIED.,.F.,.F.,
(4,2,2,2,2,2,4),(1.36970442594422,1.55800700581067,1.81772140236946,2.07743579892825,
2.33715019548703,2.59686459204582,2.78516717191228),.UNSPECIFIED.);
#231=B_SPLINE_CURVE_WITH_KNOTS('',3,(#7840,#7841,#7842,#7843,#7844,#7845,
#7846,#7847,#7848,#7849,#7850,#7851,#7852,#7853,#7854,#7855,#7856,#7857),
 .UNSPECIFIED.,.F.,.F.,(4,2,2,2,2,2,2,2,4),(0.,0.175311710953118,0.350623421906236,
0.525787580035871,0.700951738165507,0.876115896295143,1.05128005442478,
1.2265917653779,1.40190347633101),.UNSPECIFIED.);
#232=B_SPLINE_CURVE_WITH_KNOTS('',3,(#7858,#7859,#7860,#7861,#7862,#7863,
#7864,#7865,#7866,#7867,#7868,#7869,#7870,#7871,#7872,#7873,#7874,#7875),
 .UNSPECIFIED.,.F.,.F.,(4,2,2,2,2,2,2,2,4),(1.40190347633101,1.57721518728413,
1.75252689823725,1.92769105636689,2.10285521449652,2.27801937262616,2.45318353075579,
2.62849524170891,2.80380695266203),.UNSPECIFIED.);
#233=B_SPLINE_CURVE_WITH_KNOTS('',3,(#8136,#8137,#8138,#8139,#8140,#8141,
#8142,#8143,#8144,#8145,#8146,#8147,#8148,#8149,#8150,#8151,#8152,#8153,
#8154,#8155,#8156,#8157),.UNSPECIFIED.,.F.,.F.,(4,2,2,2,2,2,2,2,2,2,4),
(0.0789094028588958,0.210573405340968,0.315860108011452,0.421146810681936,
0.522142632548711,0.623138454415485,0.72413427628226,0.825130098149035,
0.930416800819519,1.03570350349,1.16736750597208),.UNSPECIFIED.);
#234=B_SPLINE_CURVE_WITH_KNOTS('',3,(#8161,#8162,#8163,#8164,#8165,#8166,
#8167,#8168,#8169,#8170,#8171,#8172,#8173,#8174,#8175,#8176,#8177,#8178,
#8179,#8180,#8181,#8182),.UNSPECIFIED.,.F.,.F.,(4,2,2,2,2,2,2,2,2,2,4),
(0.0774793363974613,0.142088896491891,0.284177792983782,0.411119756996526,
0.514392970548519,0.617666184100513,0.720939397652506,0.8242126112045,0.951154575217244,
1.09324347170913,1.15785303180356),.UNSPECIFIED.);
#235=B_SPLINE_CURVE_WITH_KNOTS('',3,(#8188,#8189,#8190,#8191,#8192,#8193,
#8194,#8195,#8196,#8197,#8198,#8199,#8200,#8201,#8202,#8203,#8204,#8205,
#8206,#8207,#8208,#8209),.UNSPECIFIED.,.F.,.F.,(4,2,2,2,2,2,2,2,2,2,4),
(0.0774793363974613,0.142088896491891,0.284177792983782,0.411119756996525,
0.514392970548519,0.617666184100513,0.720939397652506,0.8242126112045,0.951154575217243,
1.09324347170913,1.15785303180356),.UNSPECIFIED.);
#236=B_SPLINE_CURVE_WITH_KNOTS('',3,(#8213,#8214,#8215,#8216,#8217,#8218,
#8219,#8220,#8221,#8222,#8223,#8224,#8225,#8226,#8227,#8228,#8229,#8230,
#8231,#8232,#8233,#8234),.UNSPECIFIED.,.F.,.F.,(4,2,2,2,2,2,2,2,2,2,4),
(0.0774793363974614,0.142088896491891,0.284177792983781,0.411119756996525,
0.514392970548519,0.617666184100512,0.720939397652506,0.824212611204499,
0.951154575217243,1.09324347170913,1.15785303180356),.UNSPECIFIED.);
#237=B_SPLINE_CURVE_WITH_KNOTS('',3,(#8238,#8239,#8240,#8241,#8242,#8243,
#8244,#8245,#8246,#8247,#8248,#8249),.UNSPECIFIED.,.F.,.F.,(4,2,2,2,2,4),
(0.0774793363974613,0.142088896491891,0.284177792983781,0.411119756996525,
0.514392970548519,0.617666184100512),.UNSPECIFIED.);
#238=B_SPLINE_CURVE_WITH_KNOTS('',3,(#8254,#8255,#8256,#8257,#8258,#8259,
#8260,#8261,#8262,#8263,#8264,#8265),.UNSPECIFIED.,.F.,.F.,(4,2,2,2,2,4),
(0.617666184100512,0.720939397652506,0.824212611204499,0.951154575217243,
1.09324347170913,1.15785303180356),.UNSPECIFIED.);
#239=B_SPLINE_CURVE_WITH_KNOTS('',3,(#8269,#8270,#8271,#8272,#8273,#8274,
#8275,#8276,#8277,#8278,#8279,#8280,#8281,#8282,#8283,#8284,#8285,#8286,
#8287,#8288,#8289,#8290),.UNSPECIFIED.,.F.,.F.,(4,2,2,2,2,2,2,2,2,2,4),
(0.0774793363974613,0.142088896491891,0.284177792983782,0.411119756996526,
0.514392970548519,0.617666184100513,0.720939397652507,0.8242126112045,0.951154575217245,
1.09324347170914,1.15785303180356),.UNSPECIFIED.);
#240=B_SPLINE_CURVE_WITH_KNOTS('',3,(#8294,#8295,#8296,#8297,#8298,#8299,
#8300,#8301,#8302,#8303,#8304,#8305,#8306,#8307,#8308,#8309,#8310,#8311,
#8312,#8313,#8314,#8315),.UNSPECIFIED.,.F.,.F.,(4,2,2,2,2,2,2,2,2,2,4),
(0.0774793363974613,0.142088896491891,0.284177792983782,0.411119756996526,
0.514392970548519,0.617666184100513,0.720939397652506,0.824212611204499,
0.951154575217243,1.09324347170913,1.15785303180356),.UNSPECIFIED.);
#241=B_SPLINE_CURVE_WITH_KNOTS('',3,(#8319,#8320,#8321,#8322,#8323,#8324,
#8325,#8326,#8327,#8328,#8329,#8330,#8331,#8332,#8333,#8334,#8335,#8336,
#8337,#8338,#8339,#8340),.UNSPECIFIED.,.F.,.F.,(4,2,2,2,2,2,2,2,2,2,4),
(0.0774793363974613,0.142088896491891,0.284177792983782,0.411119756996526,
0.514392970548519,0.617666184100513,0.720939397652506,0.8242126112045,0.951154575217244,
1.09324347170913,1.15785303180356),.UNSPECIFIED.);
#242=B_SPLINE_CURVE_WITH_KNOTS('',3,(#8344,#8345,#8346,#8347,#8348,#8349,
#8350,#8351,#8352,#8353,#8354,#8355,#8356,#8357,#8358,#8359,#8360,#8361,
#8362,#8363,#8364,#8365),.UNSPECIFIED.,.F.,.F.,(4,2,2,2,2,2,2,2,2,2,4),
(0.0774793363974613,0.142088896491891,0.284177792983782,0.411119756996526,
0.514392970548519,0.617666184100513,0.720939397652506,0.8242126112045,0.951154575217243,
1.09324347170913,1.15785303180356),.UNSPECIFIED.);
#243=B_SPLINE_CURVE_WITH_KNOTS('',3,(#8373,#8374,#8375,#8376,#8377,#8378,
#8379,#8380,#8381,#8382,#8383,#8384,#8385,#8386,#8387,#8388,#8389,#8390,
#8391,#8392,#8393,#8394),.UNSPECIFIED.,.F.,.F.,(4,2,2,2,2,2,2,2,2,2,4),
(0.0789094028588958,0.210573405340968,0.315860108011452,0.421146810681936,
0.522142632548711,0.623138454415485,0.72413427628226,0.825130098149035,
0.930416800819519,1.03570350349,1.16736750597208),.UNSPECIFIED.);
#244=B_SPLINE_CURVE_WITH_KNOTS('',3,(#8402,#8403,#8404,#8405,#8406,#8407,
#8408,#8409,#8410,#8411,#8412,#8413,#8414,#8415,#8416,#8417,#8418,#8419,
#8420,#8421,#8422,#8423),.UNSPECIFIED.,.F.,.F.,(4,2,2,2,2,2,2,2,2,2,4),
(0.0789094028588958,0.210573405340969,0.315860108011453,0.421146810681937,
0.522142632548712,0.623138454415486,0.724134276282261,0.825130098149035,
0.930416800819519,1.03570350349,1.16736750597208),.UNSPECIFIED.);
#245=B_SPLINE_CURVE_WITH_KNOTS('',3,(#8432,#8433,#8434,#8435,#8436,#8437,
#8438,#8439,#8440,#8441,#8442,#8443),.UNSPECIFIED.,.F.,.F.,(4,2,2,2,2,4),
(0.0789094028588958,0.210573405340968,0.315860108011452,0.421146810681937,
0.522142632548711,0.623138454415486),.UNSPECIFIED.);
#246=B_SPLINE_CURVE_WITH_KNOTS('',3,(#8445,#8446,#8447,#8448,#8449,#8450,
#8451,#8452,#8453,#8454,#8455,#8456),.UNSPECIFIED.,.F.,.F.,(4,2,2,2,2,4),
(0.623138454415486,0.72413427628226,0.825130098149035,0.930416800819519,
1.03570350349,1.16736750597208),.UNSPECIFIED.);
#247=B_SPLINE_CURVE_WITH_KNOTS('',3,(#8463,#8464,#8465,#8466,#8467,#8468,
#8469,#8470,#8471,#8472,#8473,#8474,#8475,#8476,#8477,#8478,#8479,#8480,
#8481,#8482,#8483,#8484),.UNSPECIFIED.,.F.,.F.,(4,2,2,2,2,2,2,2,2,2,4),
(0.0789094028588958,0.210573405340968,0.315860108011452,0.421146810681936,
0.522142632548711,0.623138454415486,0.72413427628226,0.825130098149035,
0.930416800819519,1.03570350349,1.16736750597208),.UNSPECIFIED.);
#248=B_SPLINE_CURVE_WITH_KNOTS('',3,(#8492,#8493,#8494,#8495,#8496,#8497,
#8498,#8499,#8500,#8501,#8502,#8503,#8504,#8505,#8506,#8507,#8508,#8509,
#8510,#8511,#8512,#8513),.UNSPECIFIED.,.F.,.F.,(4,2,2,2,2,2,2,2,2,2,4),
(0.0789094028588957,0.210573405340968,0.315860108011452,0.421146810681936,
0.522142632548711,0.623138454415485,0.72413427628226,0.825130098149035,
0.930416800819519,1.03570350349,1.16736750597207),.UNSPECIFIED.);
#249=B_SPLINE_CURVE_WITH_KNOTS('',3,(#8521,#8522,#8523,#8524,#8525,#8526,
#8527,#8528,#8529,#8530,#8531,#8532,#8533,#8534,#8535,#8536,#8537,#8538,
#8539,#8540,#8541,#8542),.UNSPECIFIED.,.F.,.F.,(4,2,2,2,2,2,2,2,2,2,4),
(0.0789094028588958,0.210573405340968,0.315860108011452,0.421146810681936,
0.522142632548711,0.623138454415486,0.72413427628226,0.825130098149035,
0.930416800819519,1.03570350349,1.16736750597208),.UNSPECIFIED.);
#250=B_SPLINE_CURVE_WITH_KNOTS('',3,(#8551,#8552,#8553,#8554,#8555,#8556,
#8557,#8558,#8559,#8560,#8561,#8562,#8563,#8564,#8565,#8566,#8567,#8568,
#8569,#8570,#8571,#8572),.UNSPECIFIED.,.F.,.F.,(4,2,2,2,2,2,2,2,2,2,4),
(0.0789094028588958,0.210573405340968,0.315860108011452,0.421146810681936,
0.522142632548711,0.623138454415485,0.72413427628226,0.825130098149035,
0.930416800819519,1.03570350349,1.16736750597208),.UNSPECIFIED.);
#251=B_SPLINE_CURVE_WITH_KNOTS('',3,(#8795,#8796,#8797,#8798,#8799,#8800,
#8801,#8802,#8803,#8804,#8805,#8806,#8807,#8808,#8809,#8810,#8811,#8812),
 .UNSPECIFIED.,.F.,.F.,(4,2,2,2,2,2,2,2,4),(0.,0.113783176196775,0.22756635239355,
0.34131563198115,0.455064911568751,0.568814191156351,0.682563470743952,
0.796346646940726,0.910129823137501),.UNSPECIFIED.);
#252=B_SPLINE_CURVE_WITH_KNOTS('',3,(#8813,#8814,#8815,#8816,#8817,#8818,
#8819,#8820,#8821,#8822,#8823,#8824,#8825,#8826,#8827,#8828,#8829,#8830),
 .UNSPECIFIED.,.F.,.F.,(4,2,2,2,2,2,2,2,4),(0.910129823137501,1.02391299933428,
1.13769617553105,1.25144545511865,1.36519473470625,1.47894401429385,1.59269329388145,
1.70647647007823,1.820259646275),.UNSPECIFIED.);
#253=B_SPLINE_CURVE_WITH_KNOTS('',3,(#8865,#8866,#8867,#8868,#8869,#8870,
#8871,#8872,#8873,#8874,#8875,#8876,#8877,#8878,#8879,#8880,#8881,#8882,
#8883,#8884,#8885,#8886),.UNSPECIFIED.,.F.,.F.,(4,2,2,2,2,2,2,2,2,2,4),
(0.,0.0604340316452086,0.120868063290417,0.241736126580834,0.36006196705804,
0.478387807535245,0.596713648012451,0.715039488489656,0.835907551780074,
0.896341583425282,0.956775615070491),.UNSPECIFIED.);
#254=B_SPLINE_CURVE_WITH_KNOTS('',3,(#8887,#8888,#8889,#8890,#8891,#8892,
#8893,#8894,#8895,#8896,#8897,#8898,#8899,#8900,#8901,#8902,#8903,#8904,
#8905,#8906,#8907,#8908),.UNSPECIFIED.,.F.,.F.,(4,2,2,2,2,2,2,2,2,2,4),
(0.956775615070491,1.0172096467157,1.07764367836091,1.19851174165133,1.31683758212853,
1.43516342260574,1.55348926308294,1.67181510356015,1.79268316685056,1.85311719849577,
1.91355123014098),.UNSPECIFIED.);
#255=B_SPLINE_CURVE_WITH_KNOTS('',3,(#8940,#8941,#8942,#8943,#8944,#8945,
#8946,#8947,#8948,#8949,#8950,#8951,#8952,#8953),.UNSPECIFIED.,.F.,.F.,
(4,2,2,2,2,2,4),(0.756005737987012,0.793568827564648,0.872922520054202,
0.952276212543757,1.03162990503331,1.11098359752287,1.1485466871005),
 .UNSPECIFIED.);
#256=B_SPLINE_CURVE_WITH_KNOTS('',3,(#8959,#8960,#8961,#8962,#8963,#8964,
#8965,#8966,#8967,#8968,#8969,#8970,#8971,#8972,#8973,#8974,#8975,#8976),
 .UNSPECIFIED.,.F.,.F.,(4,2,2,2,2,2,2,2,4),(0.,0.0792165807733632,0.158433161546726,
0.237648697074571,0.316864232602415,0.396079768130259,0.475295303658103,
0.554511884431466,0.63372846520483),.UNSPECIFIED.);
#257=B_SPLINE_CURVE_WITH_KNOTS('',3,(#8977,#8978,#8979,#8980,#8981,#8982,
#8983,#8984,#8985,#8986,#8987,#8988,#8989,#8990,#8991,#8992,#8993,#8994),
 .UNSPECIFIED.,.F.,.F.,(4,2,2,2,2,2,2,2,4),(0.63372846520483,0.712945045978192,
0.792161626751555,0.8713771622794,0.950592697807244,1.02980823333509,1.10902376886293,
1.1882403496363,1.26745693040966),.UNSPECIFIED.);
#258=B_SPLINE_CURVE_WITH_KNOTS('',3,(#8997,#8998,#8999,#9000,#9001,#9002,
#9003,#9004,#9005,#9006,#9007,#9008,#9009,#9010),.UNSPECIFIED.,.F.,.F.,
(4,2,2,2,2,2,4),(0.121154929624506,0.158718019202143,0.238071711691698,
0.317425404181252,0.396779096670807,0.476132789160362,0.513695878738),
 .UNSPECIFIED.);
#259=SHAPE_REPRESENTATION_RELATIONSHIP('SRR','None',#9559,#286);
#260=SHAPE_REPRESENTATION_RELATIONSHIP('SRR','None',#9560,#287);
#261=SHAPE_REPRESENTATION_RELATIONSHIP('SRR','None',#9561,#288);
#262=SHAPE_REPRESENTATION_RELATIONSHIP('SRR','None',#9562,#289);
#263=SHAPE_REPRESENTATION_RELATIONSHIP('SRR','None',#9563,#290);
#264=SHAPE_REPRESENTATION_RELATIONSHIP('SRR','None',#9564,#291);
#265=SHAPE_REPRESENTATION_RELATIONSHIP('SRR','None',#9565,#292);
#266=SHAPE_REPRESENTATION_RELATIONSHIP('SRR','None',#9566,#293);
#267=SHAPE_REPRESENTATION_RELATIONSHIP('SRR','None',#9567,#294);
#268=SHAPE_REPRESENTATION_RELATIONSHIP('SRR','None',#9568,#295);
#269=SHAPE_REPRESENTATION_RELATIONSHIP('SRR','None',#9569,#296);
#270=SHAPE_REPRESENTATION_RELATIONSHIP('SRR','None',#9571,#297);
#271=SHAPE_REPRESENTATION_RELATIONSHIP('SRR','None',#9572,#298);
#272=SHAPE_REPRESENTATION_RELATIONSHIP('SRR','None',#9573,#299);
#273=SHAPE_REPRESENTATION_RELATIONSHIP('SRR','None',#9574,#300);
#274=SHAPE_REPRESENTATION_RELATIONSHIP('SRR','None',#9575,#301);
#275=SHAPE_REPRESENTATION_RELATIONSHIP('SRR','None',#9576,#302);
#276=SHAPE_REPRESENTATION_RELATIONSHIP('SRR','None',#9577,#303);
#277=SHAPE_REPRESENTATION_RELATIONSHIP('SRR','None',#9579,#304);
#278=SHAPE_REPRESENTATION_RELATIONSHIP('SRR','None',#9580,#305);
#279=SHAPE_REPRESENTATION_RELATIONSHIP('SRR','None',#9581,#306);
#280=SHAPE_REPRESENTATION_RELATIONSHIP('SRR','None',#9582,#307);
#281=SHAPE_REPRESENTATION_RELATIONSHIP('SRR','None',#9583,#308);
#282=SHAPE_REPRESENTATION_RELATIONSHIP('SRR','None',#9584,#309);
#283=SHAPE_REPRESENTATION_RELATIONSHIP('SRR','None',#9585,#310);
#284=SHAPE_REPRESENTATION_RELATIONSHIP('SRR','None',#9586,#311);
#285=SHAPE_REPRESENTATION_RELATIONSHIP('SRR','None',#9587,#312);
#286=ADVANCED_BREP_SHAPE_REPRESENTATION('',(#348),#9419);
#287=ADVANCED_BREP_SHAPE_REPRESENTATION('',(#349),#9420);
#288=ADVANCED_BREP_SHAPE_REPRESENTATION('',(#350),#9421);
#289=ADVANCED_BREP_SHAPE_REPRESENTATION('',(#351),#9422);
#290=ADVANCED_BREP_SHAPE_REPRESENTATION('',(#352),#9423);
#291=ADVANCED_BREP_SHAPE_REPRESENTATION('',(#353),#9424);
#292=ADVANCED_BREP_SHAPE_REPRESENTATION('',(#354),#9425);
#293=ADVANCED_BREP_SHAPE_REPRESENTATION('',(#355),#9426);
#294=ADVANCED_BREP_SHAPE_REPRESENTATION('',(#356),#9427);
#295=ADVANCED_BREP_SHAPE_REPRESENTATION('',(#357),#9428);
#296=ADVANCED_BREP_SHAPE_REPRESENTATION('',(#358),#9429);
#297=ADVANCED_BREP_SHAPE_REPRESENTATION('',(#359),#9431);
#298=ADVANCED_BREP_SHAPE_REPRESENTATION('',(#360),#9432);
#299=ADVANCED_BREP_SHAPE_REPRESENTATION('',(#361,#362,#363,#364,#365,#366,
#367,#368),#9433);
#300=ADVANCED_BREP_SHAPE_REPRESENTATION('',(#369),#9434);
#301=ADVANCED_BREP_SHAPE_REPRESENTATION('',(#370,#371),#9435);
#302=ADVANCED_BREP_SHAPE_REPRESENTATION('',(#14),#9436);
#303=ADVANCED_BREP_SHAPE_REPRESENTATION('',(#15),#9437);
#304=ADVANCED_BREP_SHAPE_REPRESENTATION('',(#372),#9439);
#305=ADVANCED_BREP_SHAPE_REPRESENTATION('',(#373),#9440);
#306=ADVANCED_BREP_SHAPE_REPRESENTATION('',(#374),#9441);
#307=ADVANCED_BREP_SHAPE_REPRESENTATION('',(#375),#9442);
#308=ADVANCED_BREP_SHAPE_REPRESENTATION('',(#376),#9443);
#309=ADVANCED_BREP_SHAPE_REPRESENTATION('',(#377),#9444);
#310=ADVANCED_BREP_SHAPE_REPRESENTATION('',(#378),#9445);
#311=ADVANCED_BREP_SHAPE_REPRESENTATION('',(#379),#9446);
#312=ADVANCED_BREP_SHAPE_REPRESENTATION('',(#16),#9447);
#313=STYLED_ITEM('',(#9757),#348);
#314=STYLED_ITEM('',(#9757),#349);
#315=STYLED_ITEM('',(#9785),#350);
#316=STYLED_ITEM('',(#9785),#351);
#317=STYLED_ITEM('',(#9785),#352);
#318=STYLED_ITEM('',(#9785),#353);
#319=STYLED_ITEM('',(#9764),#354);
#320=STYLED_ITEM('',(#9778),#355);
#321=STYLED_ITEM('',(#9778),#356);
#322=STYLED_ITEM('',(#9771),#357);
#323=STYLED_ITEM('',(#9771),#358);
#324=STYLED_ITEM('',(#9778),#359);
#325=STYLED_ITEM('',(#9778),#360);
#326=STYLED_ITEM('',(#9778),#361);
#327=STYLED_ITEM('',(#9778),#362);
#328=STYLED_ITEM('',(#9778),#363);
#329=STYLED_ITEM('',(#9778),#364);
#330=STYLED_ITEM('',(#9778),#365);
#331=STYLED_ITEM('',(#9778),#366);
#332=STYLED_ITEM('',(#9778),#367);
#333=STYLED_ITEM('',(#9778),#368);
#334=STYLED_ITEM('',(#9778),#369);
#335=STYLED_ITEM('',(#9778),#370);
#336=STYLED_ITEM('',(#9778),#371);
#337=STYLED_ITEM('',(#9785),#14);
#338=STYLED_ITEM('',(#9785),#15);
#339=STYLED_ITEM('',(#9764),#372);
#340=STYLED_ITEM('',(#9778),#373);
#341=STYLED_ITEM('',(#9778),#374);
#342=STYLED_ITEM('',(#9771),#375);
#343=STYLED_ITEM('',(#9792),#376);
#344=STYLED_ITEM('',(#9771),#377);
#345=STYLED_ITEM('',(#9785),#378);
#346=STYLED_ITEM('',(#9778),#379);
#347=STYLED_ITEM('',(#9785),#16);
#348=MANIFOLD_SOLID_BREP('Body1',#4868);
#349=MANIFOLD_SOLID_BREP('Body1',#4869);
#350=MANIFOLD_SOLID_BREP('Body1',#4870);
#351=MANIFOLD_SOLID_BREP('Body1',#4871);
#352=MANIFOLD_SOLID_BREP('Body1',#4872);
#353=MANIFOLD_SOLID_BREP('Body1',#4873);
#354=MANIFOLD_SOLID_BREP('Body1',#4874);
#355=MANIFOLD_SOLID_BREP('Body1',#4875);
#356=MANIFOLD_SOLID_BREP('Body1',#4876);
#357=MANIFOLD_SOLID_BREP('Body1',#4877);
#358=MANIFOLD_SOLID_BREP('Body1',#4878);
#359=MANIFOLD_SOLID_BREP('Body1',#4879);
#360=MANIFOLD_SOLID_BREP('Body1',#4880);
#361=MANIFOLD_SOLID_BREP('Body1',#4881);
#362=MANIFOLD_SOLID_BREP('Body2',#4882);
#363=MANIFOLD_SOLID_BREP('Body3',#4883);
#364=MANIFOLD_SOLID_BREP('Body4',#4884);
#365=MANIFOLD_SOLID_BREP('Body5',#4885);
#366=MANIFOLD_SOLID_BREP('Body6',#4886);
#367=MANIFOLD_SOLID_BREP('Body7',#4887);
#368=MANIFOLD_SOLID_BREP('Body8',#4888);
#369=MANIFOLD_SOLID_BREP('Continuous crown cage',#4889);
#370=MANIFOLD_SOLID_BREP('Body1',#4890);
#371=MANIFOLD_SOLID_BREP('Body2',#4891);
#372=MANIFOLD_SOLID_BREP('Body1',#4896);
#373=MANIFOLD_SOLID_BREP('Body1',#4897);
#374=MANIFOLD_SOLID_BREP('Body1',#4898);
#375=MANIFOLD_SOLID_BREP('Body1',#4899);
#376=MANIFOLD_SOLID_BREP('Body1',#4900);
#377=MANIFOLD_SOLID_BREP('Body1',#4901);
#378=MANIFOLD_SOLID_BREP('Body1',#4902);
#379=MANIFOLD_SOLID_BREP('Body1',#4903);
#380=FACE_BOUND('',#964,.T.);
#381=FACE_BOUND('',#965,.T.);
#382=FACE_BOUND('',#966,.T.);
#383=FACE_BOUND('',#967,.T.);
#384=FACE_BOUND('',#969,.T.);
#385=FACE_BOUND('',#970,.T.);
#386=FACE_BOUND('',#971,.T.);
#387=FACE_BOUND('',#972,.T.);
#388=FACE_BOUND('',#999,.T.);
#389=FACE_BOUND('',#1001,.T.);
#390=FACE_BOUND('',#1004,.T.);
#391=FACE_BOUND('',#1005,.T.);
#392=FACE_BOUND('',#1012,.T.);
#393=FACE_BOUND('',#1014,.T.);
#394=FACE_BOUND('',#1017,.T.);
#395=FACE_BOUND('',#1018,.T.);
#396=FACE_BOUND('',#1021,.T.);
#397=FACE_BOUND('',#1023,.T.);
#398=FACE_BOUND('',#1024,.T.);
#399=FACE_BOUND('',#1025,.T.);
#400=FACE_BOUND('',#1027,.T.);
#401=FACE_BOUND('',#1028,.T.);
#402=FACE_BOUND('',#1029,.T.);
#403=FACE_BOUND('',#1030,.T.);
#404=FACE_BOUND('',#1031,.T.);
#405=FACE_BOUND('',#1033,.T.);
#406=FACE_BOUND('',#1034,.T.);
#407=FACE_BOUND('',#1035,.T.);
#408=FACE_BOUND('',#1036,.T.);
#409=FACE_BOUND('',#1037,.T.);
#410=FACE_BOUND('',#1040,.T.);
#411=FACE_BOUND('',#1042,.T.);
#412=FACE_BOUND('',#1047,.T.);
#413=FACE_BOUND('',#1049,.T.);
#414=FACE_BOUND('',#1053,.T.);
#415=FACE_BOUND('',#1055,.T.);
#416=FACE_BOUND('',#1060,.T.);
#417=FACE_BOUND('',#1062,.T.);
#418=FACE_BOUND('',#1067,.T.);
#419=FACE_BOUND('',#1069,.T.);
#420=FACE_BOUND('',#1073,.T.);
#421=FACE_BOUND('',#1075,.T.);
#422=FACE_BOUND('',#1082,.T.);
#423=FACE_BOUND('',#1086,.T.);
#424=FACE_BOUND('',#1087,.T.);
#425=FACE_BOUND('',#1088,.T.);
#426=FACE_BOUND('',#1089,.T.);
#427=FACE_BOUND('',#1090,.T.);
#428=FACE_BOUND('',#1092,.T.);
#429=FACE_BOUND('',#1093,.T.);
#430=FACE_BOUND('',#1094,.T.);
#431=FACE_BOUND('',#1095,.T.);
#432=FACE_BOUND('',#1096,.T.);
#433=FACE_BOUND('',#1103,.T.);
#434=FACE_BOUND('',#1107,.T.);
#435=FACE_BOUND('',#1108,.T.);
#436=FACE_BOUND('',#1109,.T.);
#437=FACE_BOUND('',#1110,.T.);
#438=FACE_BOUND('',#1111,.T.);
#439=FACE_BOUND('',#1113,.T.);
#440=FACE_BOUND('',#1114,.T.);
#441=FACE_BOUND('',#1115,.T.);
#442=FACE_BOUND('',#1116,.T.);
#443=FACE_BOUND('',#1117,.T.);
#444=FACE_BOUND('',#1135,.T.);
#445=FACE_BOUND('',#1138,.T.);
#446=FACE_BOUND('',#1143,.T.);
#447=FACE_BOUND('',#1148,.T.);
#448=FACE_BOUND('',#1176,.T.);
#449=FACE_BOUND('',#1179,.T.);
#450=FACE_BOUND('',#1182,.T.);
#451=FACE_BOUND('',#1185,.T.);
#452=FACE_BOUND('',#1188,.T.);
#453=FACE_BOUND('',#1195,.T.);
#454=FACE_BOUND('',#1213,.T.);
#455=FACE_BOUND('',#1233,.T.);
#456=FACE_BOUND('',#1235,.T.);
#457=FACE_BOUND('',#1238,.T.);
#458=FACE_BOUND('',#1245,.T.);
#459=FACE_BOUND('',#1248,.T.);
#460=FACE_BOUND('',#1251,.T.);
#461=FACE_BOUND('',#1253,.T.);
#462=FACE_BOUND('',#1257,.T.);
#463=FACE_BOUND('',#1259,.T.);
#464=FACE_BOUND('',#1264,.T.);
#465=FACE_BOUND('',#1266,.T.);
#466=FACE_BOUND('',#1268,.T.);
#467=FACE_BOUND('',#1270,.T.);
#468=FACE_BOUND('',#1275,.T.);
#469=FACE_BOUND('',#1276,.T.);
#470=FACE_BOUND('',#1277,.T.);
#471=FACE_BOUND('',#1278,.T.);
#472=FACE_BOUND('',#1279,.T.);
#473=FACE_BOUND('',#1286,.T.);
#474=FACE_BOUND('',#1287,.T.);
#475=FACE_BOUND('',#1288,.T.);
#476=FACE_BOUND('',#1289,.T.);
#477=FACE_BOUND('',#1290,.T.);
#478=FACE_BOUND('',#1294,.T.);
#479=FACE_BOUND('',#1298,.T.);
#480=FACE_BOUND('',#1300,.T.);
#481=FACE_BOUND('',#1302,.T.);
#482=FACE_BOUND('',#1304,.T.);
#483=FACE_BOUND('',#1313,.T.);
#484=FACE_BOUND('',#1318,.T.);
#485=FACE_BOUND('',#1328,.T.);
#486=FACE_BOUND('',#1348,.T.);
#487=PLANE('',#5219);
#488=PLANE('',#5220);
#489=PLANE('',#5221);
#490=PLANE('',#5222);
#491=PLANE('',#5223);
#492=PLANE('',#5224);
#493=PLANE('',#5229);
#494=PLANE('',#5233);
#495=PLANE('',#5237);
#496=PLANE('',#5241);
#497=PLANE('',#5245);
#498=PLANE('',#5249);
#499=PLANE('',#5253);
#500=PLANE('',#5257);
#501=PLANE('',#5271);
#502=PLANE('',#5273);
#503=PLANE('',#5275);
#504=PLANE('',#5277);
#505=PLANE('',#5279);
#506=PLANE('',#5280);
#507=PLANE('',#5281);
#508=PLANE('',#5282);
#509=PLANE('',#5283);
#510=PLANE('',#5284);
#511=PLANE('',#5286);
#512=PLANE('',#5288);
#513=PLANE('',#5290);
#514=PLANE('',#5292);
#515=PLANE('',#5293);
#516=PLANE('',#5294);
#517=PLANE('',#5295);
#518=PLANE('',#5296);
#519=PLANE('',#5303);
#520=PLANE('',#5304);
#521=PLANE('',#5309);
#522=PLANE('',#5311);
#523=PLANE('',#5320);
#524=PLANE('',#5321);
#525=PLANE('',#5330);
#526=PLANE('',#5332);
#527=PLANE('',#5341);
#528=PLANE('',#5342);
#529=PLANE('',#5352);
#530=PLANE('',#5354);
#531=PLANE('',#5362);
#532=PLANE('',#5379);
#533=PLANE('',#5386);
#534=PLANE('',#5387);
#535=PLANE('',#5404);
#536=PLANE('',#5411);
#537=PLANE('',#5412);
#538=PLANE('',#5414);
#539=PLANE('',#5415);
#540=PLANE('',#5416);
#541=PLANE('',#5417);
#542=PLANE('',#5418);
#543=PLANE('',#5419);
#544=PLANE('',#5421);
#545=PLANE('',#5422);
#546=PLANE('',#5423);
#547=PLANE('',#5424);
#548=PLANE('',#5425);
#549=PLANE('',#5426);
#550=PLANE('',#5442);
#551=PLANE('',#5445);
#552=PLANE('',#5457);
#553=PLANE('',#5466);
#554=PLANE('',#5499);
#555=PLANE('',#5504);
#556=PLANE('',#5509);
#557=PLANE('',#5514);
#558=PLANE('',#5519);
#559=PLANE('',#5524);
#560=PLANE('',#5533);
#561=PLANE('',#5537);
#562=PLANE('',#5538);
#563=PLANE('',#5540);
#564=PLANE('',#5545);
#565=PLANE('',#5548);
#566=PLANE('',#5553);
#567=PLANE('',#5562);
#568=PLANE('',#5570);
#569=PLANE('',#5578);
#570=PLANE('',#5579);
#571=PLANE('',#5580);
#572=PLANE('',#5581);
#573=PLANE('',#5582);
#574=PLANE('',#5583);
#575=PLANE('',#5584);
#576=PLANE('',#5585);
#577=PLANE('',#5586);
#578=PLANE('',#5588);
#579=PLANE('',#5596);
#580=PLANE('',#5604);
#581=PLANE('',#5605);
#582=PLANE('',#5606);
#583=PLANE('',#5607);
#584=PLANE('',#5608);
#585=PLANE('',#5609);
#586=PLANE('',#5610);
#587=PLANE('',#5611);
#588=PLANE('',#5612);
#589=PLANE('',#5618);
#590=PLANE('',#5619);
#591=PLANE('',#5620);
#592=PLANE('',#5622);
#593=PLANE('',#5623);
#594=PLANE('',#5628);
#595=PLANE('',#5630);
#596=PLANE('',#5632);
#597=PLANE('',#5635);
#598=PLANE('',#5645);
#599=PLANE('',#5649);
#600=PLANE('',#5650);
#601=PLANE('',#5651);
#602=PLANE('',#5659);
#603=PLANE('',#5660);
#604=PLANE('',#5662);
#605=PLANE('',#5667);
#606=PLANE('',#5674);
#607=PLANE('',#5675);
#608=PLANE('',#5677);
#609=PLANE('',#5678);
#610=PLANE('',#5679);
#611=PLANE('',#5680);
#612=PLANE('',#5697);
#613=PLANE('',#5703);
#614=PLANE('',#5711);
#615=PLANE('',#5712);
#616=PLANE('',#5714);
#617=PLANE('',#5716);
#618=PLANE('',#5718);
#619=PLANE('',#5719);
#620=PLANE('',#5720);
#621=PLANE('',#5721);
#622=PLANE('',#5722);
#623=PLANE('',#5723);
#624=PLANE('',#5726);
#625=PLANE('',#5734);
#626=PLANE('',#5764);
#627=PLANE('',#5765);
#628=PLANE('',#5766);
#629=PLANE('',#5767);
#630=PLANE('',#5768);
#631=PLANE('',#5769);
#632=PLANE('',#5770);
#633=PLANE('',#5771);
#634=PLANE('',#5779);
#635=PLANE('',#5781);
#636=PLANE('',#5782);
#637=PLANE('',#5783);
#638=PLANE('',#5784);
#639=PLANE('',#5785);
#640=PLANE('',#5786);
#641=PLANE('',#5787);
#642=PLANE('',#5788);
#643=PLANE('',#5789);
#644=PLANE('',#5790);
#645=PLANE('',#5792);
#646=PLANE('',#5800);
#647=PLANE('',#5808);
#648=PLANE('',#5809);
#649=PLANE('',#5810);
#650=PLANE('',#5811);
#651=PLANE('',#5812);
#652=PLANE('',#5813);
#653=PLANE('',#5814);
#654=PLANE('',#5815);
#655=PLANE('',#5816);
#656=FACE_OUTER_BOUND('',#955,.T.);
#657=FACE_OUTER_BOUND('',#956,.T.);
#658=FACE_OUTER_BOUND('',#957,.T.);
#659=FACE_OUTER_BOUND('',#958,.T.);
#660=FACE_OUTER_BOUND('',#959,.T.);
#661=FACE_OUTER_BOUND('',#960,.T.);
#662=FACE_OUTER_BOUND('',#961,.T.);
#663=FACE_OUTER_BOUND('',#962,.T.);
#664=FACE_OUTER_BOUND('',#963,.T.);
#665=FACE_OUTER_BOUND('',#968,.T.);
#666=FACE_OUTER_BOUND('',#973,.T.);
#667=FACE_OUTER_BOUND('',#974,.T.);
#668=FACE_OUTER_BOUND('',#975,.T.);
#669=FACE_OUTER_BOUND('',#976,.T.);
#670=FACE_OUTER_BOUND('',#977,.T.);
#671=FACE_OUTER_BOUND('',#978,.T.);
#672=FACE_OUTER_BOUND('',#979,.T.);
#673=FACE_OUTER_BOUND('',#980,.T.);
#674=FACE_OUTER_BOUND('',#981,.T.);
#675=FACE_OUTER_BOUND('',#982,.T.);
#676=FACE_OUTER_BOUND('',#983,.T.);
#677=FACE_OUTER_BOUND('',#984,.T.);
#678=FACE_OUTER_BOUND('',#985,.T.);
#679=FACE_OUTER_BOUND('',#986,.T.);
#680=FACE_OUTER_BOUND('',#987,.T.);
#681=FACE_OUTER_BOUND('',#988,.T.);
#682=FACE_OUTER_BOUND('',#989,.T.);
#683=FACE_OUTER_BOUND('',#990,.T.);
#684=FACE_OUTER_BOUND('',#991,.T.);
#685=FACE_OUTER_BOUND('',#992,.T.);
#686=FACE_OUTER_BOUND('',#993,.T.);
#687=FACE_OUTER_BOUND('',#994,.T.);
#688=FACE_OUTER_BOUND('',#995,.T.);
#689=FACE_OUTER_BOUND('',#996,.T.);
#690=FACE_OUTER_BOUND('',#997,.T.);
#691=FACE_OUTER_BOUND('',#998,.T.);
#692=FACE_OUTER_BOUND('',#1000,.T.);
#693=FACE_OUTER_BOUND('',#1002,.T.);
#694=FACE_OUTER_BOUND('',#1003,.T.);
#695=FACE_OUTER_BOUND('',#1006,.T.);
#696=FACE_OUTER_BOUND('',#1007,.T.);
#697=FACE_OUTER_BOUND('',#1008,.T.);
#698=FACE_OUTER_BOUND('',#1009,.T.);
#699=FACE_OUTER_BOUND('',#1010,.T.);
#700=FACE_OUTER_BOUND('',#1011,.T.);
#701=FACE_OUTER_BOUND('',#1013,.T.);
#702=FACE_OUTER_BOUND('',#1015,.T.);
#703=FACE_OUTER_BOUND('',#1016,.T.);
#704=FACE_OUTER_BOUND('',#1019,.T.);
#705=FACE_OUTER_BOUND('',#1020,.T.);
#706=FACE_OUTER_BOUND('',#1022,.T.);
#707=FACE_OUTER_BOUND('',#1026,.T.);
#708=FACE_OUTER_BOUND('',#1032,.T.);
#709=FACE_OUTER_BOUND('',#1038,.T.);
#710=FACE_OUTER_BOUND('',#1039,.T.);
#711=FACE_OUTER_BOUND('',#1041,.T.);
#712=FACE_OUTER_BOUND('',#1043,.T.);
#713=FACE_OUTER_BOUND('',#1044,.T.);
#714=FACE_OUTER_BOUND('',#1045,.T.);
#715=FACE_OUTER_BOUND('',#1046,.T.);
#716=FACE_OUTER_BOUND('',#1048,.T.);
#717=FACE_OUTER_BOUND('',#1050,.T.);
#718=FACE_OUTER_BOUND('',#1051,.T.);
#719=FACE_OUTER_BOUND('',#1052,.T.);
#720=FACE_OUTER_BOUND('',#1054,.T.);
#721=FACE_OUTER_BOUND('',#1056,.T.);
#722=FACE_OUTER_BOUND('',#1057,.T.);
#723=FACE_OUTER_BOUND('',#1058,.T.);
#724=FACE_OUTER_BOUND('',#1059,.T.);
#725=FACE_OUTER_BOUND('',#1061,.T.);
#726=FACE_OUTER_BOUND('',#1063,.T.);
#727=FACE_OUTER_BOUND('',#1064,.T.);
#728=FACE_OUTER_BOUND('',#1065,.T.);
#729=FACE_OUTER_BOUND('',#1066,.T.);
#730=FACE_OUTER_BOUND('',#1068,.T.);
#731=FACE_OUTER_BOUND('',#1070,.T.);
#732=FACE_OUTER_BOUND('',#1071,.T.);
#733=FACE_OUTER_BOUND('',#1072,.T.);
#734=FACE_OUTER_BOUND('',#1074,.T.);
#735=FACE_OUTER_BOUND('',#1076,.T.);
#736=FACE_OUTER_BOUND('',#1077,.T.);
#737=FACE_OUTER_BOUND('',#1078,.T.);
#738=FACE_OUTER_BOUND('',#1079,.T.);
#739=FACE_OUTER_BOUND('',#1080,.T.);
#740=FACE_OUTER_BOUND('',#1081,.T.);
#741=FACE_OUTER_BOUND('',#1083,.T.);
#742=FACE_OUTER_BOUND('',#1084,.T.);
#743=FACE_OUTER_BOUND('',#1085,.T.);
#744=FACE_OUTER_BOUND('',#1091,.T.);
#745=FACE_OUTER_BOUND('',#1097,.T.);
#746=FACE_OUTER_BOUND('',#1098,.T.);
#747=FACE_OUTER_BOUND('',#1099,.T.);
#748=FACE_OUTER_BOUND('',#1100,.T.);
#749=FACE_OUTER_BOUND('',#1101,.T.);
#750=FACE_OUTER_BOUND('',#1102,.T.);
#751=FACE_OUTER_BOUND('',#1104,.T.);
#752=FACE_OUTER_BOUND('',#1105,.T.);
#753=FACE_OUTER_BOUND('',#1106,.T.);
#754=FACE_OUTER_BOUND('',#1112,.T.);
#755=FACE_OUTER_BOUND('',#1118,.T.);
#756=FACE_OUTER_BOUND('',#1119,.T.);
#757=FACE_OUTER_BOUND('',#1120,.T.);
#758=FACE_OUTER_BOUND('',#1121,.T.);
#759=FACE_OUTER_BOUND('',#1122,.T.);
#760=FACE_OUTER_BOUND('',#1123,.T.);
#761=FACE_OUTER_BOUND('',#1124,.T.);
#762=FACE_OUTER_BOUND('',#1125,.T.);
#763=FACE_OUTER_BOUND('',#1126,.T.);
#764=FACE_OUTER_BOUND('',#1127,.T.);
#765=FACE_OUTER_BOUND('',#1128,.T.);
#766=FACE_OUTER_BOUND('',#1129,.T.);
#767=FACE_OUTER_BOUND('',#1130,.T.);
#768=FACE_OUTER_BOUND('',#1131,.T.);
#769=FACE_OUTER_BOUND('',#1132,.T.);
#770=FACE_OUTER_BOUND('',#1133,.T.);
#771=FACE_OUTER_BOUND('',#1134,.T.);
#772=FACE_OUTER_BOUND('',#1136,.T.);
#773=FACE_OUTER_BOUND('',#1137,.T.);
#774=FACE_OUTER_BOUND('',#1139,.T.);
#775=FACE_OUTER_BOUND('',#1140,.T.);
#776=FACE_OUTER_BOUND('',#1141,.T.);
#777=FACE_OUTER_BOUND('',#1142,.T.);
#778=FACE_OUTER_BOUND('',#1144,.T.);
#779=FACE_OUTER_BOUND('',#1145,.T.);
#780=FACE_OUTER_BOUND('',#1146,.T.);
#781=FACE_OUTER_BOUND('',#1147,.T.);
#782=FACE_OUTER_BOUND('',#1149,.T.);
#783=FACE_OUTER_BOUND('',#1150,.T.);
#784=FACE_OUTER_BOUND('',#1151,.T.);
#785=FACE_OUTER_BOUND('',#1152,.T.);
#786=FACE_OUTER_BOUND('',#1153,.T.);
#787=FACE_OUTER_BOUND('',#1154,.T.);
#788=FACE_OUTER_BOUND('',#1155,.T.);
#789=FACE_OUTER_BOUND('',#1156,.T.);
#790=FACE_OUTER_BOUND('',#1157,.T.);
#791=FACE_OUTER_BOUND('',#1158,.T.);
#792=FACE_OUTER_BOUND('',#1159,.T.);
#793=FACE_OUTER_BOUND('',#1160,.T.);
#794=FACE_OUTER_BOUND('',#1161,.T.);
#795=FACE_OUTER_BOUND('',#1162,.T.);
#796=FACE_OUTER_BOUND('',#1163,.T.);
#797=FACE_OUTER_BOUND('',#1164,.T.);
#798=FACE_OUTER_BOUND('',#1165,.T.);
#799=FACE_OUTER_BOUND('',#1166,.T.);
#800=FACE_OUTER_BOUND('',#1167,.T.);
#801=FACE_OUTER_BOUND('',#1168,.T.);
#802=FACE_OUTER_BOUND('',#1169,.T.);
#803=FACE_OUTER_BOUND('',#1170,.T.);
#804=FACE_OUTER_BOUND('',#1171,.T.);
#805=FACE_OUTER_BOUND('',#1172,.T.);
#806=FACE_OUTER_BOUND('',#1173,.T.);
#807=FACE_OUTER_BOUND('',#1174,.T.);
#808=FACE_OUTER_BOUND('',#1175,.T.);
#809=FACE_OUTER_BOUND('',#1177,.T.);
#810=FACE_OUTER_BOUND('',#1178,.T.);
#811=FACE_OUTER_BOUND('',#1180,.T.);
#812=FACE_OUTER_BOUND('',#1181,.T.);
#813=FACE_OUTER_BOUND('',#1183,.T.);
#814=FACE_OUTER_BOUND('',#1184,.T.);
#815=FACE_OUTER_BOUND('',#1186,.T.);
#816=FACE_OUTER_BOUND('',#1187,.T.);
#817=FACE_OUTER_BOUND('',#1189,.T.);
#818=FACE_OUTER_BOUND('',#1190,.T.);
#819=FACE_OUTER_BOUND('',#1191,.T.);
#820=FACE_OUTER_BOUND('',#1192,.T.);
#821=FACE_OUTER_BOUND('',#1193,.T.);
#822=FACE_OUTER_BOUND('',#1194,.T.);
#823=FACE_OUTER_BOUND('',#1196,.T.);
#824=FACE_OUTER_BOUND('',#1197,.T.);
#825=FACE_OUTER_BOUND('',#1198,.T.);
#826=FACE_OUTER_BOUND('',#1199,.T.);
#827=FACE_OUTER_BOUND('',#1200,.T.);
#828=FACE_OUTER_BOUND('',#1201,.T.);
#829=FACE_OUTER_BOUND('',#1202,.T.);
#830=FACE_OUTER_BOUND('',#1203,.T.);
#831=FACE_OUTER_BOUND('',#1204,.T.);
#832=FACE_OUTER_BOUND('',#1205,.T.);
#833=FACE_OUTER_BOUND('',#1206,.T.);
#834=FACE_OUTER_BOUND('',#1207,.T.);
#835=FACE_OUTER_BOUND('',#1208,.T.);
#836=FACE_OUTER_BOUND('',#1209,.T.);
#837=FACE_OUTER_BOUND('',#1210,.T.);
#838=FACE_OUTER_BOUND('',#1211,.T.);
#839=FACE_OUTER_BOUND('',#1212,.T.);
#840=FACE_OUTER_BOUND('',#1214,.T.);
#841=FACE_OUTER_BOUND('',#1215,.T.);
#842=FACE_OUTER_BOUND('',#1216,.T.);
#843=FACE_OUTER_BOUND('',#1217,.T.);
#844=FACE_OUTER_BOUND('',#1218,.T.);
#845=FACE_OUTER_BOUND('',#1219,.T.);
#846=FACE_OUTER_BOUND('',#1220,.T.);
#847=FACE_OUTER_BOUND('',#1221,.T.);
#848=FACE_OUTER_BOUND('',#1222,.T.);
#849=FACE_OUTER_BOUND('',#1223,.T.);
#850=FACE_OUTER_BOUND('',#1224,.T.);
#851=FACE_OUTER_BOUND('',#1225,.T.);
#852=FACE_OUTER_BOUND('',#1226,.T.);
#853=FACE_OUTER_BOUND('',#1227,.T.);
#854=FACE_OUTER_BOUND('',#1228,.T.);
#855=FACE_OUTER_BOUND('',#1229,.T.);
#856=FACE_OUTER_BOUND('',#1230,.T.);
#857=FACE_OUTER_BOUND('',#1231,.T.);
#858=FACE_OUTER_BOUND('',#1232,.T.);
#859=FACE_OUTER_BOUND('',#1234,.T.);
#860=FACE_OUTER_BOUND('',#1236,.T.);
#861=FACE_OUTER_BOUND('',#1237,.T.);
#862=FACE_OUTER_BOUND('',#1239,.T.);
#863=FACE_OUTER_BOUND('',#1240,.T.);
#864=FACE_OUTER_BOUND('',#1241,.T.);
#865=FACE_OUTER_BOUND('',#1242,.T.);
#866=FACE_OUTER_BOUND('',#1243,.T.);
#867=FACE_OUTER_BOUND('',#1244,.T.);
#868=FACE_OUTER_BOUND('',#1246,.T.);
#869=FACE_OUTER_BOUND('',#1247,.T.);
#870=FACE_OUTER_BOUND('',#1249,.T.);
#871=FACE_OUTER_BOUND('',#1250,.T.);
#872=FACE_OUTER_BOUND('',#1252,.T.);
#873=FACE_OUTER_BOUND('',#1254,.T.);
#874=FACE_OUTER_BOUND('',#1255,.T.);
#875=FACE_OUTER_BOUND('',#1256,.T.);
#876=FACE_OUTER_BOUND('',#1258,.T.);
#877=FACE_OUTER_BOUND('',#1260,.T.);
#878=FACE_OUTER_BOUND('',#1261,.T.);
#879=FACE_OUTER_BOUND('',#1262,.T.);
#880=FACE_OUTER_BOUND('',#1263,.T.);
#881=FACE_OUTER_BOUND('',#1265,.T.);
#882=FACE_OUTER_BOUND('',#1267,.T.);
#883=FACE_OUTER_BOUND('',#1269,.T.);
#884=FACE_OUTER_BOUND('',#1271,.T.);
#885=FACE_OUTER_BOUND('',#1272,.T.);
#886=FACE_OUTER_BOUND('',#1273,.T.);
#887=FACE_OUTER_BOUND('',#1274,.T.);
#888=FACE_OUTER_BOUND('',#1280,.T.);
#889=FACE_OUTER_BOUND('',#1281,.T.);
#890=FACE_OUTER_BOUND('',#1282,.T.);
#891=FACE_OUTER_BOUND('',#1283,.T.);
#892=FACE_OUTER_BOUND('',#1284,.T.);
#893=FACE_OUTER_BOUND('',#1285,.T.);
#894=FACE_OUTER_BOUND('',#1291,.T.);
#895=FACE_OUTER_BOUND('',#1292,.T.);
#896=FACE_OUTER_BOUND('',#1293,.T.);
#897=FACE_OUTER_BOUND('',#1295,.T.);
#898=FACE_OUTER_BOUND('',#1296,.T.);
#899=FACE_OUTER_BOUND('',#1297,.T.);
#900=FACE_OUTER_BOUND('',#1299,.T.);
#901=FACE_OUTER_BOUND('',#1301,.T.);
#902=FACE_OUTER_BOUND('',#1303,.T.);
#903=FACE_OUTER_BOUND('',#1305,.T.);
#904=FACE_OUTER_BOUND('',#1306,.T.);
#905=FACE_OUTER_BOUND('',#1307,.T.);
#906=FACE_OUTER_BOUND('',#1308,.T.);
#907=FACE_OUTER_BOUND('',#1309,.T.);
#908=FACE_OUTER_BOUND('',#1310,.T.);
#909=FACE_OUTER_BOUND('',#1311,.T.);
#910=FACE_OUTER_BOUND('',#1312,.T.);
#911=FACE_OUTER_BOUND('',#1314,.T.);
#912=FACE_OUTER_BOUND('',#1315,.T.);
#913=FACE_OUTER_BOUND('',#1316,.T.);
#914=FACE_OUTER_BOUND('',#1317,.T.);
#915=FACE_OUTER_BOUND('',#1319,.T.);
#916=FACE_OUTER_BOUND('',#1320,.T.);
#917=FACE_OUTER_BOUND('',#1321,.T.);
#918=FACE_OUTER_BOUND('',#1322,.T.);
#919=FACE_OUTER_BOUND('',#1323,.T.);
#920=FACE_OUTER_BOUND('',#1324,.T.);
#921=FACE_OUTER_BOUND('',#1325,.T.);
#922=FACE_OUTER_BOUND('',#1326,.T.);
#923=FACE_OUTER_BOUND('',#1327,.T.);
#924=FACE_OUTER_BOUND('',#1329,.T.);
#925=FACE_OUTER_BOUND('',#1330,.T.);
#926=FACE_OUTER_BOUND('',#1331,.T.);
#927=FACE_OUTER_BOUND('',#1332,.T.);
#928=FACE_OUTER_BOUND('',#1333,.T.);
#929=FACE_OUTER_BOUND('',#1334,.T.);
#930=FACE_OUTER_BOUND('',#1335,.T.);
#931=FACE_OUTER_BOUND('',#1336,.T.);
#932=FACE_OUTER_BOUND('',#1337,.T.);
#933=FACE_OUTER_BOUND('',#1338,.T.);
#934=FACE_OUTER_BOUND('',#1339,.T.);
#935=FACE_OUTER_BOUND('',#1340,.T.);
#936=FACE_OUTER_BOUND('',#1341,.T.);
#937=FACE_OUTER_BOUND('',#1342,.T.);
#938=FACE_OUTER_BOUND('',#1343,.T.);
#939=FACE_OUTER_BOUND('',#1344,.T.);
#940=FACE_OUTER_BOUND('',#1345,.T.);
#941=FACE_OUTER_BOUND('',#1346,.T.);
#942=FACE_OUTER_BOUND('',#1347,.T.);
#943=FACE_OUTER_BOUND('',#1349,.T.);
#944=FACE_OUTER_BOUND('',#1350,.T.);
#945=FACE_OUTER_BOUND('',#1351,.T.);
#946=FACE_OUTER_BOUND('',#1352,.T.);
#947=FACE_OUTER_BOUND('',#1353,.T.);
#948=FACE_OUTER_BOUND('',#1354,.T.);
#949=FACE_OUTER_BOUND('',#1355,.T.);
#950=FACE_OUTER_BOUND('',#1356,.T.);
#951=FACE_OUTER_BOUND('',#1357,.T.);
#952=FACE_OUTER_BOUND('',#1358,.T.);
#953=FACE_OUTER_BOUND('',#1359,.T.);
#954=FACE_OUTER_BOUND('',#1360,.T.);
#955=EDGE_LOOP('',(#3267,#3268,#3269,#3270));
#956=EDGE_LOOP('',(#3271,#3272,#3273,#3274));
#957=EDGE_LOOP('',(#3275,#3276,#3277,#3278));
#958=EDGE_LOOP('',(#3279,#3280,#3281,#3282));
#959=EDGE_LOOP('',(#3283,#3284,#3285,#3286));
#960=EDGE_LOOP('',(#3287,#3288,#3289,#3290));
#961=EDGE_LOOP('',(#3291,#3292,#3293,#3294));
#962=EDGE_LOOP('',(#3295,#3296,#3297,#3298));
#963=EDGE_LOOP('',(#3299,#3300,#3301,#3302));
#964=EDGE_LOOP('',(#3303));
#965=EDGE_LOOP('',(#3304));
#966=EDGE_LOOP('',(#3305));
#967=EDGE_LOOP('',(#3306));
#968=EDGE_LOOP('',(#3307,#3308,#3309,#3310));
#969=EDGE_LOOP('',(#3311));
#970=EDGE_LOOP('',(#3312));
#971=EDGE_LOOP('',(#3313));
#972=EDGE_LOOP('',(#3314));
#973=EDGE_LOOP('',(#3315,#3316,#3317,#3318));
#974=EDGE_LOOP('',(#3319));
#975=EDGE_LOOP('',(#3320,#3321,#3322,#3323));
#976=EDGE_LOOP('',(#3324));
#977=EDGE_LOOP('',(#3325,#3326,#3327,#3328));
#978=EDGE_LOOP('',(#3329));
#979=EDGE_LOOP('',(#3330,#3331,#3332,#3333));
#980=EDGE_LOOP('',(#3334));
#981=EDGE_LOOP('',(#3335,#3336,#3337,#3338));
#982=EDGE_LOOP('',(#3339));
#983=EDGE_LOOP('',(#3340,#3341,#3342,#3343));
#984=EDGE_LOOP('',(#3344));
#985=EDGE_LOOP('',(#3345,#3346,#3347,#3348));
#986=EDGE_LOOP('',(#3349));
#987=EDGE_LOOP('',(#3350,#3351,#3352,#3353));
#988=EDGE_LOOP('',(#3354));
#989=EDGE_LOOP('',(#3355,#3356,#3357,#3358,#3359,#3360));
#990=EDGE_LOOP('',(#3361,#3362,#3363,#3364));
#991=EDGE_LOOP('',(#3365,#3366,#3367,#3368));
#992=EDGE_LOOP('',(#3369,#3370,#3371,#3372));
#993=EDGE_LOOP('',(#3373,#3374,#3375,#3376));
#994=EDGE_LOOP('',(#3377,#3378,#3379,#3380));
#995=EDGE_LOOP('',(#3381,#3382,#3383,#3384));
#996=EDGE_LOOP('',(#3385,#3386,#3387,#3388));
#997=EDGE_LOOP('',(#3389,#3390,#3391,#3392));
#998=EDGE_LOOP('',(#3393,#3394,#3395,#3396));
#999=EDGE_LOOP('',(#3397));
#1000=EDGE_LOOP('',(#3398,#3399,#3400,#3401));
#1001=EDGE_LOOP('',(#3402));
#1002=EDGE_LOOP('',(#3403,#3404,#3405,#3406));
#1003=EDGE_LOOP('',(#3407,#3408,#3409,#3410,#3411,#3412));
#1004=EDGE_LOOP('',(#3413));
#1005=EDGE_LOOP('',(#3414));
#1006=EDGE_LOOP('',(#3415,#3416,#3417,#3418));
#1007=EDGE_LOOP('',(#3419,#3420,#3421,#3422));
#1008=EDGE_LOOP('',(#3423,#3424,#3425,#3426));
#1009=EDGE_LOOP('',(#3427,#3428,#3429,#3430));
#1010=EDGE_LOOP('',(#3431,#3432,#3433,#3434));
#1011=EDGE_LOOP('',(#3435,#3436,#3437,#3438));
#1012=EDGE_LOOP('',(#3439));
#1013=EDGE_LOOP('',(#3440,#3441,#3442,#3443));
#1014=EDGE_LOOP('',(#3444));
#1015=EDGE_LOOP('',(#3445,#3446,#3447,#3448));
#1016=EDGE_LOOP('',(#3449,#3450,#3451,#3452,#3453,#3454));
#1017=EDGE_LOOP('',(#3455));
#1018=EDGE_LOOP('',(#3456));
#1019=EDGE_LOOP('',(#3457,#3458,#3459,#3460));
#1020=EDGE_LOOP('',(#3461,#3462,#3463,#3464));
#1021=EDGE_LOOP('',(#3465,#3466));
#1022=EDGE_LOOP('',(#3467,#3468,#3469,#3470));
#1023=EDGE_LOOP('',(#3471,#3472));
#1024=EDGE_LOOP('',(#3473,#3474,#3475,#3476,#3477,#3478));
#1025=EDGE_LOOP('',(#3479,#3480,#3481,#3482,#3483,#3484));
#1026=EDGE_LOOP('',(#3485));
#1027=EDGE_LOOP('',(#3486));
#1028=EDGE_LOOP('',(#3487));
#1029=EDGE_LOOP('',(#3488));
#1030=EDGE_LOOP('',(#3489));
#1031=EDGE_LOOP('',(#3490));
#1032=EDGE_LOOP('',(#3491));
#1033=EDGE_LOOP('',(#3492));
#1034=EDGE_LOOP('',(#3493));
#1035=EDGE_LOOP('',(#3494));
#1036=EDGE_LOOP('',(#3495));
#1037=EDGE_LOOP('',(#3496));
#1038=EDGE_LOOP('',(#3497,#3498,#3499,#3500));
#1039=EDGE_LOOP('',(#3501));
#1040=EDGE_LOOP('',(#3502));
#1041=EDGE_LOOP('',(#3503));
#1042=EDGE_LOOP('',(#3504));
#1043=EDGE_LOOP('',(#3505,#3506,#3507,#3508));
#1044=EDGE_LOOP('',(#3509,#3510,#3511,#3512));
#1045=EDGE_LOOP('',(#3513,#3514,#3515,#3516));
#1046=EDGE_LOOP('',(#3517));
#1047=EDGE_LOOP('',(#3518));
#1048=EDGE_LOOP('',(#3519));
#1049=EDGE_LOOP('',(#3520));
#1050=EDGE_LOOP('',(#3521,#3522,#3523,#3524));
#1051=EDGE_LOOP('',(#3525,#3526,#3527,#3528));
#1052=EDGE_LOOP('',(#3529));
#1053=EDGE_LOOP('',(#3530));
#1054=EDGE_LOOP('',(#3531));
#1055=EDGE_LOOP('',(#3532));
#1056=EDGE_LOOP('',(#3533,#3534,#3535,#3536));
#1057=EDGE_LOOP('',(#3537,#3538,#3539,#3540));
#1058=EDGE_LOOP('',(#3541,#3542,#3543,#3544));
#1059=EDGE_LOOP('',(#3545));
#1060=EDGE_LOOP('',(#3546));
#1061=EDGE_LOOP('',(#3547));
#1062=EDGE_LOOP('',(#3548));
#1063=EDGE_LOOP('',(#3549,#3550,#3551,#3552));
#1064=EDGE_LOOP('',(#3553,#3554,#3555,#3556));
#1065=EDGE_LOOP('',(#3557,#3558,#3559,#3560));
#1066=EDGE_LOOP('',(#3561,#3562,#3563,#3564));
#1067=EDGE_LOOP('',(#3565));
#1068=EDGE_LOOP('',(#3566,#3567,#3568,#3569));
#1069=EDGE_LOOP('',(#3570));
#1070=EDGE_LOOP('',(#3571,#3572,#3573,#3574));
#1071=EDGE_LOOP('',(#3575,#3576,#3577,#3578,#3579));
#1072=EDGE_LOOP('',(#3580,#3581,#3582,#3583));
#1073=EDGE_LOOP('',(#3584,#3585));
#1074=EDGE_LOOP('',(#3586,#3587,#3588,#3589));
#1075=EDGE_LOOP('',(#3590));
#1076=EDGE_LOOP('',(#3591,#3592,#3593,#3594));
#1077=EDGE_LOOP('',(#3595,#3596,#3597,#3598));
#1078=EDGE_LOOP('',(#3599,#3600,#3601,#3602));
#1079=EDGE_LOOP('',(#3603,#3604,#3605,#3606));
#1080=EDGE_LOOP('',(#3607,#3608,#3609,#3610));
#1081=EDGE_LOOP('',(#3611));
#1082=EDGE_LOOP('',(#3612));
#1083=EDGE_LOOP('',(#3613,#3614,#3615,#3616));
#1084=EDGE_LOOP('',(#3617,#3618,#3619,#3620));
#1085=EDGE_LOOP('',(#3621));
#1086=EDGE_LOOP('',(#3622));
#1087=EDGE_LOOP('',(#3623));
#1088=EDGE_LOOP('',(#3624));
#1089=EDGE_LOOP('',(#3625));
#1090=EDGE_LOOP('',(#3626));
#1091=EDGE_LOOP('',(#3627));
#1092=EDGE_LOOP('',(#3628));
#1093=EDGE_LOOP('',(#3629));
#1094=EDGE_LOOP('',(#3630));
#1095=EDGE_LOOP('',(#3631));
#1096=EDGE_LOOP('',(#3632));
#1097=EDGE_LOOP('',(#3633,#3634,#3635,#3636));
#1098=EDGE_LOOP('',(#3637,#3638,#3639,#3640));
#1099=EDGE_LOOP('',(#3641,#3642,#3643,#3644));
#1100=EDGE_LOOP('',(#3645,#3646,#3647,#3648));
#1101=EDGE_LOOP('',(#3649,#3650,#3651,#3652));
#1102=EDGE_LOOP('',(#3653));
#1103=EDGE_LOOP('',(#3654));
#1104=EDGE_LOOP('',(#3655,#3656,#3657,#3658));
#1105=EDGE_LOOP('',(#3659,#3660,#3661,#3662));
#1106=EDGE_LOOP('',(#3663));
#1107=EDGE_LOOP('',(#3664));
#1108=EDGE_LOOP('',(#3665));
#1109=EDGE_LOOP('',(#3666));
#1110=EDGE_LOOP('',(#3667));
#1111=EDGE_LOOP('',(#3668));
#1112=EDGE_LOOP('',(#3669));
#1113=EDGE_LOOP('',(#3670));
#1114=EDGE_LOOP('',(#3671));
#1115=EDGE_LOOP('',(#3672));
#1116=EDGE_LOOP('',(#3673));
#1117=EDGE_LOOP('',(#3674));
#1118=EDGE_LOOP('',(#3675,#3676,#3677,#3678));
#1119=EDGE_LOOP('',(#3679,#3680,#3681,#3682));
#1120=EDGE_LOOP('',(#3683,#3684,#3685,#3686));
#1121=EDGE_LOOP('',(#3687,#3688,#3689,#3690));
#1122=EDGE_LOOP('',(#3691,#3692,#3693,#3694));
#1123=EDGE_LOOP('',(#3695,#3696,#3697,#3698));
#1124=EDGE_LOOP('',(#3699,#3700,#3701,#3702));
#1125=EDGE_LOOP('',(#3703,#3704,#3705,#3706));
#1126=EDGE_LOOP('',(#3707,#3708,#3709,#3710));
#1127=EDGE_LOOP('',(#3711,#3712,#3713,#3714));
#1128=EDGE_LOOP('',(#3715,#3716,#3717,#3718));
#1129=EDGE_LOOP('',(#3719,#3720,#3721,#3722));
#1130=EDGE_LOOP('',(#3723,#3724,#3725,#3726,#3727,#3728));
#1131=EDGE_LOOP('',(#3729,#3730,#3731,#3732,#3733));
#1132=EDGE_LOOP('',(#3734,#3735,#3736,#3737));
#1133=EDGE_LOOP('',(#3738,#3739,#3740,#3741));
#1134=EDGE_LOOP('',(#3742));
#1135=EDGE_LOOP('',(#3743));
#1136=EDGE_LOOP('',(#3744,#3745,#3746,#3747,#3748));
#1137=EDGE_LOOP('',(#3749));
#1138=EDGE_LOOP('',(#3750));
#1139=EDGE_LOOP('',(#3751,#3752,#3753,#3754));
#1140=EDGE_LOOP('',(#3755,#3756,#3757,#3758,#3759,#3760));
#1141=EDGE_LOOP('',(#3761,#3762,#3763,#3764,#3765));
#1142=EDGE_LOOP('',(#3766));
#1143=EDGE_LOOP('',(#3767));
#1144=EDGE_LOOP('',(#3768,#3769,#3770,#3771));
#1145=EDGE_LOOP('',(#3772,#3773,#3774,#3775));
#1146=EDGE_LOOP('',(#3776,#3777,#3778,#3779));
#1147=EDGE_LOOP('',(#3780));
#1148=EDGE_LOOP('',(#3781));
#1149=EDGE_LOOP('',(#3782,#3783,#3784,#3785,#3786));
#1150=EDGE_LOOP('',(#3787,#3788));
#1151=EDGE_LOOP('',(#3789,#3790));
#1152=EDGE_LOOP('',(#3791,#3792));
#1153=EDGE_LOOP('',(#3793,#3794));
#1154=EDGE_LOOP('',(#3795,#3796));
#1155=EDGE_LOOP('',(#3797,#3798));
#1156=EDGE_LOOP('',(#3799,#3800));
#1157=EDGE_LOOP('',(#3801,#3802));
#1158=EDGE_LOOP('',(#3803,#3804,#3805,#3806));
#1159=EDGE_LOOP('',(#3807,#3808,#3809,#3810,#3811,#3812,#3813,#3814,#3815,
#3816,#3817,#3818,#3819,#3820,#3821,#3822,#3823,#3824,#3825,#3826));
#1160=EDGE_LOOP('',(#3827,#3828,#3829,#3830));
#1161=EDGE_LOOP('',(#3831,#3832,#3833,#3834));
#1162=EDGE_LOOP('',(#3835,#3836,#3837,#3838));
#1163=EDGE_LOOP('',(#3839,#3840,#3841,#3842));
#1164=EDGE_LOOP('',(#3843,#3844,#3845,#3846));
#1165=EDGE_LOOP('',(#3847,#3848,#3849,#3850,#3851,#3852));
#1166=EDGE_LOOP('',(#3853,#3854,#3855,#3856));
#1167=EDGE_LOOP('',(#3857,#3858,#3859,#3860));
#1168=EDGE_LOOP('',(#3861,#3862,#3863,#3864));
#1169=EDGE_LOOP('',(#3865,#3866,#3867,#3868));
#1170=EDGE_LOOP('',(#3869,#3870,#3871,#3872));
#1171=EDGE_LOOP('',(#3873,#3874,#3875,#3876));
#1172=EDGE_LOOP('',(#3877,#3878,#3879,#3880,#3881,#3882,#3883,#3884,#3885,
#3886,#3887,#3888,#3889,#3890,#3891,#3892,#3893,#3894,#3895,#3896));
#1173=EDGE_LOOP('',(#3897,#3898,#3899,#3900));
#1174=EDGE_LOOP('',(#3901,#3902,#3903,#3904));
#1175=EDGE_LOOP('',(#3905));
#1176=EDGE_LOOP('',(#3906));
#1177=EDGE_LOOP('',(#3907,#3908,#3909,#3910));
#1178=EDGE_LOOP('',(#3911));
#1179=EDGE_LOOP('',(#3912));
#1180=EDGE_LOOP('',(#3913,#3914,#3915,#3916));
#1181=EDGE_LOOP('',(#3917));
#1182=EDGE_LOOP('',(#3918));
#1183=EDGE_LOOP('',(#3919,#3920,#3921,#3922));
#1184=EDGE_LOOP('',(#3923));
#1185=EDGE_LOOP('',(#3924));
#1186=EDGE_LOOP('',(#3925,#3926,#3927,#3928));
#1187=EDGE_LOOP('',(#3929));
#1188=EDGE_LOOP('',(#3930));
#1189=EDGE_LOOP('',(#3931,#3932,#3933,#3934));
#1190=EDGE_LOOP('',(#3935));
#1191=EDGE_LOOP('',(#3936,#3937,#3938,#3939));
#1192=EDGE_LOOP('',(#3940,#3941,#3942,#3943));
#1193=EDGE_LOOP('',(#3944,#3945,#3946,#3947));
#1194=EDGE_LOOP('',(#3948));
#1195=EDGE_LOOP('',(#3949));
#1196=EDGE_LOOP('',(#3950,#3951,#3952,#3953));
#1197=EDGE_LOOP('',(#3954,#3955,#3956,#3957));
#1198=EDGE_LOOP('',(#3958,#3959,#3960,#3961));
#1199=EDGE_LOOP('',(#3962));
#1200=EDGE_LOOP('',(#3963,#3964,#3965,#3966));
#1201=EDGE_LOOP('',(#3967,#3968,#3969,#3970));
#1202=EDGE_LOOP('',(#3971,#3972,#3973,#3974));
#1203=EDGE_LOOP('',(#3975,#3976,#3977,#3978));
#1204=EDGE_LOOP('',(#3979,#3980,#3981,#3982));
#1205=EDGE_LOOP('',(#3983,#3984,#3985,#3986));
#1206=EDGE_LOOP('',(#3987,#3988,#3989,#3990,#3991,#3992));
#1207=EDGE_LOOP('',(#3993,#3994,#3995,#3996,#3997,#3998));
#1208=EDGE_LOOP('',(#3999));
#1209=EDGE_LOOP('',(#4000,#4001,#4002,#4003));
#1210=EDGE_LOOP('',(#4004,#4005,#4006,#4007));
#1211=EDGE_LOOP('',(#4008,#4009,#4010,#4011));
#1212=EDGE_LOOP('',(#4012));
#1213=EDGE_LOOP('',(#4013));
#1214=EDGE_LOOP('',(#4014,#4015,#4016,#4017));
#1215=EDGE_LOOP('',(#4018,#4019,#4020,#4021));
#1216=EDGE_LOOP('',(#4022,#4023,#4024,#4025));
#1217=EDGE_LOOP('',(#4026));
#1218=EDGE_LOOP('',(#4027,#4028,#4029,#4030));
#1219=EDGE_LOOP('',(#4031,#4032,#4033,#4034));
#1220=EDGE_LOOP('',(#4035,#4036,#4037,#4038));
#1221=EDGE_LOOP('',(#4039,#4040,#4041,#4042));
#1222=EDGE_LOOP('',(#4043,#4044,#4045,#4046));
#1223=EDGE_LOOP('',(#4047,#4048,#4049,#4050));
#1224=EDGE_LOOP('',(#4051,#4052,#4053,#4054,#4055,#4056));
#1225=EDGE_LOOP('',(#4057,#4058,#4059,#4060,#4061,#4062));
#1226=EDGE_LOOP('',(#4063,#4064,#4065,#4066));
#1227=EDGE_LOOP('',(#4067));
#1228=EDGE_LOOP('',(#4068,#4069,#4070,#4071));
#1229=EDGE_LOOP('',(#4072,#4073,#4074,#4075));
#1230=EDGE_LOOP('',(#4076,#4077,#4078,#4079));
#1231=EDGE_LOOP('',(#4080,#4081,#4082,#4083));
#1232=EDGE_LOOP('',(#4084,#4085,#4086,#4087,#4088,#4089,#4090,#4091));
#1233=EDGE_LOOP('',(#4092,#4093));
#1234=EDGE_LOOP('',(#4094));
#1235=EDGE_LOOP('',(#4095));
#1236=EDGE_LOOP('',(#4096));
#1237=EDGE_LOOP('',(#4097));
#1238=EDGE_LOOP('',(#4098));
#1239=EDGE_LOOP('',(#4099));
#1240=EDGE_LOOP('',(#4100,#4101,#4102,#4103));
#1241=EDGE_LOOP('',(#4104,#4105,#4106,#4107));
#1242=EDGE_LOOP('',(#4108,#4109,#4110,#4111));
#1243=EDGE_LOOP('',(#4112,#4113,#4114,#4115));
#1244=EDGE_LOOP('',(#4116));
#1245=EDGE_LOOP('',(#4117));
#1246=EDGE_LOOP('',(#4118,#4119,#4120,#4121,#4122,#4123));
#1247=EDGE_LOOP('',(#4124,#4125,#4126,#4127));
#1248=EDGE_LOOP('',(#4128,#4129));
#1249=EDGE_LOOP('',(#4130));
#1250=EDGE_LOOP('',(#4131,#4132,#4133,#4134,#4135));
#1251=EDGE_LOOP('',(#4136));
#1252=EDGE_LOOP('',(#4137));
#1253=EDGE_LOOP('',(#4138));
#1254=EDGE_LOOP('',(#4139,#4140,#4141,#4142));
#1255=EDGE_LOOP('',(#4143,#4144,#4145,#4146));
#1256=EDGE_LOOP('',(#4147));
#1257=EDGE_LOOP('',(#4148));
#1258=EDGE_LOOP('',(#4149));
#1259=EDGE_LOOP('',(#4150));
#1260=EDGE_LOOP('',(#4151,#4152));
#1261=EDGE_LOOP('',(#4153,#4154,#4155,#4156,#4157,#4158,#4159,#4160,#4161));
#1262=EDGE_LOOP('',(#4162,#4163,#4164));
#1263=EDGE_LOOP('',(#4165,#4166,#4167,#4168));
#1264=EDGE_LOOP('',(#4169,#4170,#4171,#4172));
#1265=EDGE_LOOP('',(#4173,#4174,#4175,#4176));
#1266=EDGE_LOOP('',(#4177,#4178));
#1267=EDGE_LOOP('',(#4179));
#1268=EDGE_LOOP('',(#4180));
#1269=EDGE_LOOP('',(#4181));
#1270=EDGE_LOOP('',(#4182));
#1271=EDGE_LOOP('',(#4183,#4184,#4185,#4186));
#1272=EDGE_LOOP('',(#4187,#4188,#4189,#4190));
#1273=EDGE_LOOP('',(#4191,#4192,#4193,#4194));
#1274=EDGE_LOOP('',(#4195));
#1275=EDGE_LOOP('',(#4196));
#1276=EDGE_LOOP('',(#4197));
#1277=EDGE_LOOP('',(#4198));
#1278=EDGE_LOOP('',(#4199));
#1279=EDGE_LOOP('',(#4200,#4201,#4202,#4203));
#1280=EDGE_LOOP('',(#4204,#4205,#4206,#4207));
#1281=EDGE_LOOP('',(#4208,#4209,#4210,#4211));
#1282=EDGE_LOOP('',(#4212,#4213,#4214,#4215));
#1283=EDGE_LOOP('',(#4216,#4217,#4218,#4219));
#1284=EDGE_LOOP('',(#4220,#4221,#4222,#4223));
#1285=EDGE_LOOP('',(#4224));
#1286=EDGE_LOOP('',(#4225));
#1287=EDGE_LOOP('',(#4226));
#1288=EDGE_LOOP('',(#4227));
#1289=EDGE_LOOP('',(#4228));
#1290=EDGE_LOOP('',(#4229));
#1291=EDGE_LOOP('',(#4230,#4231,#4232,#4233));
#1292=EDGE_LOOP('',(#4234,#4235,#4236,#4237));
#1293=EDGE_LOOP('',(#4238));
#1294=EDGE_LOOP('',(#4239,#4240,#4241,#4242));
#1295=EDGE_LOOP('',(#4243,#4244,#4245,#4246));
#1296=EDGE_LOOP('',(#4247,#4248,#4249,#4250));
#1297=EDGE_LOOP('',(#4251));
#1298=EDGE_LOOP('',(#4252));
#1299=EDGE_LOOP('',(#4253));
#1300=EDGE_LOOP('',(#4254));
#1301=EDGE_LOOP('',(#4255,#4256,#4257,#4258,#4259,#4260));
#1302=EDGE_LOOP('',(#4261));
#1303=EDGE_LOOP('',(#4262,#4263,#4264,#4265,#4266,#4267));
#1304=EDGE_LOOP('',(#4268));
#1305=EDGE_LOOP('',(#4269,#4270,#4271,#4272));
#1306=EDGE_LOOP('',(#4273,#4274,#4275,#4276));
#1307=EDGE_LOOP('',(#4277,#4278,#4279,#4280));
#1308=EDGE_LOOP('',(#4281,#4282,#4283,#4284));
#1309=EDGE_LOOP('',(#4285,#4286,#4287,#4288));
#1310=EDGE_LOOP('',(#4289,#4290,#4291,#4292));
#1311=EDGE_LOOP('',(#4293,#4294,#4295,#4296));
#1312=EDGE_LOOP('',(#4297));
#1313=EDGE_LOOP('',(#4298));
#1314=EDGE_LOOP('',(#4299,#4300,#4301,#4302));
#1315=EDGE_LOOP('',(#4303,#4304,#4305,#4306));
#1316=EDGE_LOOP('',(#4307,#4308,#4309,#4310));
#1317=EDGE_LOOP('',(#4311));
#1318=EDGE_LOOP('',(#4312));
#1319=EDGE_LOOP('',(#4313,#4314,#4315,#4316));
#1320=EDGE_LOOP('',(#4317,#4318,#4319,#4320));
#1321=EDGE_LOOP('',(#4321,#4322,#4323,#4324));
#1322=EDGE_LOOP('',(#4325,#4326,#4327,#4328));
#1323=EDGE_LOOP('',(#4329,#4330,#4331,#4332));
#1324=EDGE_LOOP('',(#4333,#4334,#4335,#4336));
#1325=EDGE_LOOP('',(#4337,#4338,#4339,#4340));
#1326=EDGE_LOOP('',(#4341,#4342,#4343,#4344,#4345,#4346));
#1327=EDGE_LOOP('',(#4347));
#1328=EDGE_LOOP('',(#4348,#4349,#4350,#4351,#4352,#4353));
#1329=EDGE_LOOP('',(#4354,#4355,#4356,#4357));
#1330=EDGE_LOOP('',(#4358,#4359,#4360,#4361));
#1331=EDGE_LOOP('',(#4362,#4363,#4364,#4365));
#1332=EDGE_LOOP('',(#4366));
#1333=EDGE_LOOP('',(#4367,#4368,#4369,#4370,#4371,#4372,#4373,#4374));
#1334=EDGE_LOOP('',(#4375,#4376,#4377,#4378));
#1335=EDGE_LOOP('',(#4379,#4380,#4381,#4382));
#1336=EDGE_LOOP('',(#4383,#4384,#4385,#4386));
#1337=EDGE_LOOP('',(#4387,#4388,#4389,#4390));
#1338=EDGE_LOOP('',(#4391,#4392,#4393,#4394,#4395,#4396,#4397,#4398));
#1339=EDGE_LOOP('',(#4399,#4400,#4401,#4402));
#1340=EDGE_LOOP('',(#4403,#4404,#4405,#4406));
#1341=EDGE_LOOP('',(#4407,#4408,#4409,#4410));
#1342=EDGE_LOOP('',(#4411,#4412,#4413,#4414));
#1343=EDGE_LOOP('',(#4415));
#1344=EDGE_LOOP('',(#4416,#4417,#4418,#4419));
#1345=EDGE_LOOP('',(#4420,#4421,#4422,#4423));
#1346=EDGE_LOOP('',(#4424,#4425,#4426,#4427));
#1347=EDGE_LOOP('',(#4428));
#1348=EDGE_LOOP('',(#4429));
#1349=EDGE_LOOP('',(#4430,#4431,#4432,#4433));
#1350=EDGE_LOOP('',(#4434,#4435,#4436,#4437));
#1351=EDGE_LOOP('',(#4438,#4439,#4440,#4441));
#1352=EDGE_LOOP('',(#4442));
#1353=EDGE_LOOP('',(#4443,#4444,#4445,#4446));
#1354=EDGE_LOOP('',(#4447,#4448,#4449,#4450));
#1355=EDGE_LOOP('',(#4451,#4452,#4453,#4454));
#1356=EDGE_LOOP('',(#4455,#4456,#4457,#4458));
#1357=EDGE_LOOP('',(#4459,#4460,#4461,#4462));
#1358=EDGE_LOOP('',(#4463,#4464,#4465,#4466));
#1359=EDGE_LOOP('',(#4467,#4468,#4469,#4470,#4471,#4472));
#1360=EDGE_LOOP('',(#4473,#4474,#4475,#4476,#4477,#4478));
#1361=LINE('',#7403,#1681);
#1362=LINE('',#7409,#1682);
#1363=LINE('',#7415,#1683);
#1364=LINE('',#7421,#1684);
#1365=LINE('',#7426,#1685);
#1366=LINE('',#7428,#1686);
#1367=LINE('',#7430,#1687);
#1368=LINE('',#7431,#1688);
#1369=LINE('',#7434,#1689);
#1370=LINE('',#7436,#1690);
#1371=LINE('',#7437,#1691);
#1372=LINE('',#7440,#1692);
#1373=LINE('',#7442,#1693);
#1374=LINE('',#7443,#1694);
#1375=LINE('',#7445,#1695);
#1376=LINE('',#7446,#1696);
#1377=LINE('',#7454,#1697);
#1378=LINE('',#7461,#1698);
#1379=LINE('',#7468,#1699);
#1380=LINE('',#7475,#1700);
#1381=LINE('',#7482,#1701);
#1382=LINE('',#7489,#1702);
#1383=LINE('',#7496,#1703);
#1384=LINE('',#7503,#1704);
#1385=LINE('',#7546,#1705);
#1386=LINE('',#7588,#1706);
#1387=LINE('',#7594,#1707);
#1388=LINE('',#7600,#1708);
#1389=LINE('',#7606,#1709);
#1390=LINE('',#7613,#1710);
#1391=LINE('',#7615,#1711);
#1392=LINE('',#7616,#1712);
#1393=LINE('',#7621,#1713);
#1394=LINE('',#7623,#1714);
#1395=LINE('',#7624,#1715);
#1396=LINE('',#7630,#1716);
#1397=LINE('',#7632,#1717);
#1398=LINE('',#7633,#1718);
#1399=LINE('',#7638,#1719);
#1400=LINE('',#7640,#1720);
#1401=LINE('',#7641,#1721);
#1402=LINE('',#7643,#1722);
#1403=LINE('',#7644,#1723);
#1404=LINE('',#7646,#1724);
#1405=LINE('',#7647,#1725);
#1406=LINE('',#7649,#1726);
#1407=LINE('',#7651,#1727);
#1408=LINE('',#7658,#1728);
#1409=LINE('',#7660,#1729);
#1410=LINE('',#7661,#1730);
#1411=LINE('',#7666,#1731);
#1412=LINE('',#7668,#1732);
#1413=LINE('',#7669,#1733);
#1414=LINE('',#7675,#1734);
#1415=LINE('',#7677,#1735);
#1416=LINE('',#7678,#1736);
#1417=LINE('',#7683,#1737);
#1418=LINE('',#7685,#1738);
#1419=LINE('',#7686,#1739);
#1420=LINE('',#7688,#1740);
#1421=LINE('',#7689,#1741);
#1422=LINE('',#7691,#1742);
#1423=LINE('',#7692,#1743);
#1424=LINE('',#7694,#1744);
#1425=LINE('',#7696,#1745);
#1426=LINE('',#7702,#1746);
#1427=LINE('',#7708,#1747);
#1428=LINE('',#7717,#1748);
#1429=LINE('',#7727,#1749);
#1430=LINE('',#7732,#1750);
#1431=LINE('',#7737,#1751);
#1432=LINE('',#7751,#1752);
#1433=LINE('',#7761,#1753);
#1434=LINE('',#7766,#1754);
#1435=LINE('',#7771,#1755);
#1436=LINE('',#7784,#1756);
#1437=LINE('',#7802,#1757);
#1438=LINE('',#7807,#1758);
#1439=LINE('',#7811,#1759);
#1440=LINE('',#7827,#1760);
#1441=LINE('',#7828,#1761);
#1442=LINE('',#7876,#1762);
#1443=LINE('',#7879,#1763);
#1444=LINE('',#7887,#1764);
#1445=LINE('',#7893,#1765);
#1446=LINE('',#7899,#1766);
#1447=LINE('',#7905,#1767);
#1448=LINE('',#7911,#1768);
#1449=LINE('',#7918,#1769);
#1450=LINE('',#7924,#1770);
#1451=LINE('',#7933,#1771);
#1452=LINE('',#7939,#1772);
#1453=LINE('',#7945,#1773);
#1454=LINE('',#7951,#1774);
#1455=LINE('',#7957,#1775);
#1456=LINE('',#7965,#1776);
#1457=LINE('',#7970,#1777);
#1458=LINE('',#7978,#1778);
#1459=LINE('',#7980,#1779);
#1460=LINE('',#7982,#1780);
#1461=LINE('',#7983,#1781);
#1462=LINE('',#7986,#1782);
#1463=LINE('',#7988,#1783);
#1464=LINE('',#7989,#1784);
#1465=LINE('',#7992,#1785);
#1466=LINE('',#7994,#1786);
#1467=LINE('',#7995,#1787);
#1468=LINE('',#7997,#1788);
#1469=LINE('',#7998,#1789);
#1470=LINE('',#8005,#1790);
#1471=LINE('',#8007,#1791);
#1472=LINE('',#8009,#1792);
#1473=LINE('',#8010,#1793);
#1474=LINE('',#8013,#1794);
#1475=LINE('',#8015,#1795);
#1476=LINE('',#8016,#1796);
#1477=LINE('',#8019,#1797);
#1478=LINE('',#8021,#1798);
#1479=LINE('',#8022,#1799);
#1480=LINE('',#8024,#1800);
#1481=LINE('',#8025,#1801);
#1482=LINE('',#8042,#1802);
#1483=LINE('',#8048,#1803);
#1484=LINE('',#8052,#1804);
#1485=LINE('',#8058,#1805);
#1486=LINE('',#8063,#1806);
#1487=LINE('',#8078,#1807);
#1488=LINE('',#8087,#1808);
#1489=LINE('',#8091,#1809);
#1490=LINE('',#8095,#1810);
#1491=LINE('',#8098,#1811);
#1492=LINE('',#8251,#1812);
#1493=LINE('',#8547,#1813);
#1494=LINE('',#8589,#1814);
#1495=LINE('',#8594,#1815);
#1496=LINE('',#8603,#1816);
#1497=LINE('',#8608,#1817);
#1498=LINE('',#8621,#1818);
#1499=LINE('',#8625,#1819);
#1500=LINE('',#8629,#1820);
#1501=LINE('',#8636,#1821);
#1502=LINE('',#8640,#1822);
#1503=LINE('',#8644,#1823);
#1504=LINE('',#8649,#1824);
#1505=LINE('',#8651,#1825);
#1506=LINE('',#8653,#1826);
#1507=LINE('',#8654,#1827);
#1508=LINE('',#8657,#1828);
#1509=LINE('',#8659,#1829);
#1510=LINE('',#8660,#1830);
#1511=LINE('',#8663,#1831);
#1512=LINE('',#8665,#1832);
#1513=LINE('',#8666,#1833);
#1514=LINE('',#8669,#1834);
#1515=LINE('',#8671,#1835);
#1516=LINE('',#8672,#1836);
#1517=LINE('',#8675,#1837);
#1518=LINE('',#8677,#1838);
#1519=LINE('',#8678,#1839);
#1520=LINE('',#8680,#1840);
#1521=LINE('',#8681,#1841);
#1522=LINE('',#8691,#1842);
#1523=LINE('',#8695,#1843);
#1524=LINE('',#8699,#1844);
#1525=LINE('',#8706,#1845);
#1526=LINE('',#8710,#1846);
#1527=LINE('',#8714,#1847);
#1528=LINE('',#8719,#1848);
#1529=LINE('',#8721,#1849);
#1530=LINE('',#8723,#1850);
#1531=LINE('',#8724,#1851);
#1532=LINE('',#8727,#1852);
#1533=LINE('',#8729,#1853);
#1534=LINE('',#8730,#1854);
#1535=LINE('',#8733,#1855);
#1536=LINE('',#8735,#1856);
#1537=LINE('',#8736,#1857);
#1538=LINE('',#8739,#1858);
#1539=LINE('',#8741,#1859);
#1540=LINE('',#8742,#1860);
#1541=LINE('',#8745,#1861);
#1542=LINE('',#8747,#1862);
#1543=LINE('',#8748,#1863);
#1544=LINE('',#8750,#1864);
#1545=LINE('',#8751,#1865);
#1546=LINE('',#8760,#1866);
#1547=LINE('',#8766,#1867);
#1548=LINE('',#8768,#1868);
#1549=LINE('',#8770,#1869);
#1550=LINE('',#8771,#1870);
#1551=LINE('',#8776,#1871);
#1552=LINE('',#8777,#1872);
#1553=LINE('',#8780,#1873);
#1554=LINE('',#8782,#1874);
#1555=LINE('',#8783,#1875);
#1556=LINE('',#8785,#1876);
#1557=LINE('',#8790,#1877);
#1558=LINE('',#8846,#1878);
#1559=LINE('',#8850,#1879);
#1560=LINE('',#8853,#1880);
#1561=LINE('',#8859,#1881);
#1562=LINE('',#8909,#1882);
#1563=LINE('',#8912,#1883);
#1564=LINE('',#8922,#1884);
#1565=LINE('',#8928,#1885);
#1566=LINE('',#8936,#1886);
#1567=LINE('',#8957,#1887);
#1568=LINE('',#9012,#1888);
#1569=LINE('',#9017,#1889);
#1570=LINE('',#9023,#1890);
#1571=LINE('',#9031,#1891);
#1572=LINE('',#9033,#1892);
#1573=LINE('',#9035,#1893);
#1574=LINE('',#9036,#1894);
#1575=LINE('',#9039,#1895);
#1576=LINE('',#9041,#1896);
#1577=LINE('',#9042,#1897);
#1578=LINE('',#9045,#1898);
#1579=LINE('',#9047,#1899);
#1580=LINE('',#9048,#1900);
#1581=LINE('',#9066,#1901);
#1582=LINE('',#9070,#1902);
#1583=LINE('',#9074,#1903);
#1584=LINE('',#9078,#1904);
#1585=LINE('',#9085,#1905);
#1586=LINE('',#9088,#1906);
#1587=LINE('',#9096,#1907);
#1588=LINE('',#9102,#1908);
#1589=LINE('',#9110,#1909);
#1590=LINE('',#9112,#1910);
#1591=LINE('',#9114,#1911);
#1592=LINE('',#9116,#1912);
#1593=LINE('',#9118,#1913);
#1594=LINE('',#9119,#1914);
#1595=LINE('',#9125,#1915);
#1596=LINE('',#9127,#1916);
#1597=LINE('',#9129,#1917);
#1598=LINE('',#9131,#1918);
#1599=LINE('',#9133,#1919);
#1600=LINE('',#9134,#1920);
#1601=LINE('',#9138,#1921);
#1602=LINE('',#9139,#1922);
#1603=LINE('',#9141,#1923);
#1604=LINE('',#9143,#1924);
#1605=LINE('',#9145,#1925);
#1606=LINE('',#9147,#1926);
#1607=LINE('',#9151,#1927);
#1608=LINE('',#9159,#1928);
#1609=LINE('',#9163,#1929);
#1610=LINE('',#9167,#1930);
#1611=LINE('',#9172,#1931);
#1612=LINE('',#9203,#1932);
#1613=LINE('',#9205,#1933);
#1614=LINE('',#9207,#1934);
#1615=LINE('',#9208,#1935);
#1616=LINE('',#9211,#1936);
#1617=LINE('',#9213,#1937);
#1618=LINE('',#9214,#1938);
#1619=LINE('',#9217,#1939);
#1620=LINE('',#9219,#1940);
#1621=LINE('',#9220,#1941);
#1622=LINE('',#9223,#1942);
#1623=LINE('',#9225,#1943);
#1624=LINE('',#9226,#1944);
#1625=LINE('',#9229,#1945);
#1626=LINE('',#9231,#1946);
#1627=LINE('',#9232,#1947);
#1628=LINE('',#9234,#1948);
#1629=LINE('',#9235,#1949);
#1630=LINE('',#9243,#1950);
#1631=LINE('',#9247,#1951);
#1632=LINE('',#9251,#1952);
#1633=LINE('',#9257,#1953);
#1634=LINE('',#9259,#1954);
#1635=LINE('',#9261,#1955);
#1636=LINE('',#9263,#1956);
#1637=LINE('',#9265,#1957);
#1638=LINE('',#9267,#1958);
#1639=LINE('',#9269,#1959);
#1640=LINE('',#9270,#1960);
#1641=LINE('',#9273,#1961);
#1642=LINE('',#9275,#1962);
#1643=LINE('',#9276,#1963);
#1644=LINE('',#9279,#1964);
#1645=LINE('',#9280,#1965);
#1646=LINE('',#9283,#1966);
#1647=LINE('',#9284,#1967);
#1648=LINE('',#9287,#1968);
#1649=LINE('',#9288,#1969);
#1650=LINE('',#9292,#1970);
#1651=LINE('',#9293,#1971);
#1652=LINE('',#9295,#1972);
#1653=LINE('',#9296,#1973);
#1654=LINE('',#9298,#1974);
#1655=LINE('',#9300,#1975);
#1656=LINE('',#9302,#1976);
#1657=LINE('',#9311,#1977);
#1658=LINE('',#9315,#1978);
#1659=LINE('',#9319,#1979);
#1660=LINE('',#9326,#1980);
#1661=LINE('',#9330,#1981);
#1662=LINE('',#9334,#1982);
#1663=LINE('',#9339,#1983);
#1664=LINE('',#9341,#1984);
#1665=LINE('',#9343,#1985);
#1666=LINE('',#9344,#1986);
#1667=LINE('',#9347,#1987);
#1668=LINE('',#9349,#1988);
#1669=LINE('',#9350,#1989);
#1670=LINE('',#9353,#1990);
#1671=LINE('',#9355,#1991);
#1672=LINE('',#9356,#1992);
#1673=LINE('',#9359,#1993);
#1674=LINE('',#9361,#1994);
#1675=LINE('',#9362,#1995);
#1676=LINE('',#9365,#1996);
#1677=LINE('',#9367,#1997);
#1678=LINE('',#9368,#1998);
#1679=LINE('',#9370,#1999);
#1680=LINE('',#9371,#2000);
#1681=VECTOR('',#5838,0.25);
#1682=VECTOR('',#5845,0.25);
#1683=VECTOR('',#5852,0.25);
#1684=VECTOR('',#5859,0.25);
#1685=VECTOR('',#5864,1.);
#1686=VECTOR('',#5865,1.);
#1687=VECTOR('',#5866,1.);
#1688=VECTOR('',#5867,1.);
#1689=VECTOR('',#5870,1.);
#1690=VECTOR('',#5871,1.);
#1691=VECTOR('',#5872,1.);
#1692=VECTOR('',#5875,1.);
#1693=VECTOR('',#5876,1.);
#1694=VECTOR('',#5877,1.);
#1695=VECTOR('',#5880,1.);
#1696=VECTOR('',#5881,1.);
#1697=VECTOR('',#5892,0.165);
#1698=VECTOR('',#5901,0.165);
#1699=VECTOR('',#5910,0.165);
#1700=VECTOR('',#5919,0.165);
#1701=VECTOR('',#5928,0.165);
#1702=VECTOR('',#5937,0.165);
#1703=VECTOR('',#5946,0.165);
#1704=VECTOR('',#5955,0.165);
#1705=VECTOR('',#5962,0.685);
#1706=VECTOR('',#5967,0.33);
#1707=VECTOR('',#5974,0.33);
#1708=VECTOR('',#5981,0.33);
#1709=VECTOR('',#5988,0.33);
#1710=VECTOR('',#5995,1.);
#1711=VECTOR('',#5996,1.);
#1712=VECTOR('',#5997,1.);
#1713=VECTOR('',#6002,1.);
#1714=VECTOR('',#6003,1.);
#1715=VECTOR('',#6004,1.);
#1716=VECTOR('',#6009,1.);
#1717=VECTOR('',#6010,1.);
#1718=VECTOR('',#6011,1.);
#1719=VECTOR('',#6016,1.);
#1720=VECTOR('',#6017,1.);
#1721=VECTOR('',#6018,1.);
#1722=VECTOR('',#6021,1.);
#1723=VECTOR('',#6022,1.);
#1724=VECTOR('',#6025,1.);
#1725=VECTOR('',#6026,1.);
#1726=VECTOR('',#6029,1.);
#1727=VECTOR('',#6032,1.);
#1728=VECTOR('',#6039,1.);
#1729=VECTOR('',#6040,1.);
#1730=VECTOR('',#6041,1.);
#1731=VECTOR('',#6046,1.);
#1732=VECTOR('',#6047,1.);
#1733=VECTOR('',#6048,1.);
#1734=VECTOR('',#6053,1.);
#1735=VECTOR('',#6054,1.);
#1736=VECTOR('',#6055,1.);
#1737=VECTOR('',#6060,1.);
#1738=VECTOR('',#6061,1.);
#1739=VECTOR('',#6062,1.);
#1740=VECTOR('',#6065,1.);
#1741=VECTOR('',#6066,1.);
#1742=VECTOR('',#6069,1.);
#1743=VECTOR('',#6070,1.);
#1744=VECTOR('',#6073,1.);
#1745=VECTOR('',#6076,1.);
#1746=VECTOR('',#6083,2.35);
#1747=VECTOR('',#6090,3.5);
#1748=VECTOR('',#6103,1.16);
#1749=VECTOR('',#6116,1.005);
#1750=VECTOR('',#6123,1.005);
#1751=VECTOR('',#6128,2.34);
#1752=VECTOR('',#6149,1.16);
#1753=VECTOR('',#6162,1.005);
#1754=VECTOR('',#6169,1.005);
#1755=VECTOR('',#6174,2.34);
#1756=VECTOR('',#6193,1.);
#1757=VECTOR('',#6194,1.);
#1758=VECTOR('',#6199,1.);
#1759=VECTOR('',#6202,1.);
#1760=VECTOR('',#6205,1.);
#1761=VECTOR('',#6206,1.);
#1762=VECTOR('',#6221,0.46);
#1763=VECTOR('',#6224,1.2);
#1764=VECTOR('',#6235,0.225);
#1765=VECTOR('',#6242,0.225);
#1766=VECTOR('',#6249,0.225);
#1767=VECTOR('',#6256,0.225);
#1768=VECTOR('',#6263,2.34);
#1769=VECTOR('',#6272,1.8);
#1770=VECTOR('',#6279,3.5);
#1771=VECTOR('',#6292,0.225);
#1772=VECTOR('',#6299,0.225);
#1773=VECTOR('',#6306,0.225);
#1774=VECTOR('',#6313,0.225);
#1775=VECTOR('',#6320,2.34);
#1776=VECTOR('',#6331,1.8);
#1777=VECTOR('',#6336,3.5);
#1778=VECTOR('',#6347,1.);
#1779=VECTOR('',#6348,1.);
#1780=VECTOR('',#6349,1.);
#1781=VECTOR('',#6350,1.);
#1782=VECTOR('',#6353,1.);
#1783=VECTOR('',#6354,1.);
#1784=VECTOR('',#6355,1.);
#1785=VECTOR('',#6358,1.);
#1786=VECTOR('',#6359,1.);
#1787=VECTOR('',#6360,1.);
#1788=VECTOR('',#6363,1.);
#1789=VECTOR('',#6364,1.);
#1790=VECTOR('',#6373,1.);
#1791=VECTOR('',#6374,1.);
#1792=VECTOR('',#6375,1.);
#1793=VECTOR('',#6376,1.);
#1794=VECTOR('',#6379,1.);
#1795=VECTOR('',#6380,1.);
#1796=VECTOR('',#6381,1.);
#1797=VECTOR('',#6384,1.);
#1798=VECTOR('',#6385,1.);
#1799=VECTOR('',#6386,1.);
#1800=VECTOR('',#6389,1.);
#1801=VECTOR('',#6390,1.);
#1802=VECTOR('',#6413,1.63531);
#1803=VECTOR('',#6420,1.);
#1804=VECTOR('',#6425,1.05);
#1805=VECTOR('',#6434,1.63531);
#1806=VECTOR('',#6441,1.05);
#1807=VECTOR('',#6460,1.71469);
#1808=VECTOR('',#6471,2.3);
#1809=VECTOR('',#6476,2.35);
#1810=VECTOR('',#6481,2.3);
#1811=VECTOR('',#6486,1.71469);
#1812=VECTOR('',#6537,1.706752);
#1813=VECTOR('',#6614,1.643248);
#1814=VECTOR('',#6643,1.70469);
#1815=VECTOR('',#6650,1.65031);
#1816=VECTOR('',#6661,1.70469);
#1817=VECTOR('',#6668,1.65031);
#1818=VECTOR('',#6689,0.475);
#1819=VECTOR('',#6694,0.5);
#1820=VECTOR('',#6699,0.485);
#1821=VECTOR('',#6708,0.31);
#1822=VECTOR('',#6713,0.3);
#1823=VECTOR('',#6718,0.27);
#1824=VECTOR('',#6723,1.);
#1825=VECTOR('',#6724,1.);
#1826=VECTOR('',#6725,1.);
#1827=VECTOR('',#6726,1.);
#1828=VECTOR('',#6729,1.);
#1829=VECTOR('',#6730,1.);
#1830=VECTOR('',#6731,1.);
#1831=VECTOR('',#6734,1.);
#1832=VECTOR('',#6735,1.);
#1833=VECTOR('',#6736,1.);
#1834=VECTOR('',#6739,1.);
#1835=VECTOR('',#6740,1.);
#1836=VECTOR('',#6741,1.);
#1837=VECTOR('',#6744,1.);
#1838=VECTOR('',#6745,1.);
#1839=VECTOR('',#6746,1.);
#1840=VECTOR('',#6749,1.);
#1841=VECTOR('',#6750,1.);
#1842=VECTOR('',#6765,0.325);
#1843=VECTOR('',#6770,0.35);
#1844=VECTOR('',#6775,0.335);
#1845=VECTOR('',#6784,0.21);
#1846=VECTOR('',#6789,0.2);
#1847=VECTOR('',#6794,0.18);
#1848=VECTOR('',#6799,1.);
#1849=VECTOR('',#6800,1.);
#1850=VECTOR('',#6801,1.);
#1851=VECTOR('',#6802,1.);
#1852=VECTOR('',#6805,1.);
#1853=VECTOR('',#6806,1.);
#1854=VECTOR('',#6807,1.);
#1855=VECTOR('',#6810,1.);
#1856=VECTOR('',#6811,1.);
#1857=VECTOR('',#6812,1.);
#1858=VECTOR('',#6815,1.);
#1859=VECTOR('',#6816,1.);
#1860=VECTOR('',#6817,1.);
#1861=VECTOR('',#6820,1.);
#1862=VECTOR('',#6821,1.);
#1863=VECTOR('',#6822,1.);
#1864=VECTOR('',#6825,1.);
#1865=VECTOR('',#6826,1.);
#1866=VECTOR('',#6839,0.21);
#1867=VECTOR('',#6846,1.);
#1868=VECTOR('',#6847,1.);
#1869=VECTOR('',#6848,1.);
#1870=VECTOR('',#6849,1.);
#1871=VECTOR('',#6854,1.);
#1872=VECTOR('',#6855,1.);
#1873=VECTOR('',#6858,1.);
#1874=VECTOR('',#6859,1.);
#1875=VECTOR('',#6860,1.);
#1876=VECTOR('',#6863,1.);
#1877=VECTOR('',#6868,1.);
#1878=VECTOR('',#6893,1.2);
#1879=VECTOR('',#6898,0.4);
#1880=VECTOR('',#6901,1.);
#1881=VECTOR('',#6908,0.685);
#1882=VECTOR('',#6915,0.3);
#1883=VECTOR('',#6918,0.4);
#1884=VECTOR('',#6933,1.005);
#1885=VECTOR('',#6940,1.35);
#1886=VECTOR('',#6951,1.);
#1887=VECTOR('',#6958,0.21);
#1888=VECTOR('',#6963,1.);
#1889=VECTOR('',#6968,1.005);
#1890=VECTOR('',#6975,1.5);
#1891=VECTOR('',#6986,1.);
#1892=VECTOR('',#6987,1.);
#1893=VECTOR('',#6988,1.);
#1894=VECTOR('',#6989,1.);
#1895=VECTOR('',#6992,1.);
#1896=VECTOR('',#6993,1.);
#1897=VECTOR('',#6994,1.);
#1898=VECTOR('',#6997,1.);
#1899=VECTOR('',#6998,1.);
#1900=VECTOR('',#6999,1.);
#1901=VECTOR('',#7022,0.275);
#1902=VECTOR('',#7027,0.275);
#1903=VECTOR('',#7032,0.275);
#1904=VECTOR('',#7037,0.275);
#1905=VECTOR('',#7046,3.);
#1906=VECTOR('',#7049,1.6);
#1907=VECTOR('',#7060,0.275);
#1908=VECTOR('',#7067,1.2);
#1909=VECTOR('',#7078,1.);
#1910=VECTOR('',#7079,1.);
#1911=VECTOR('',#7080,1.);
#1912=VECTOR('',#7081,1.);
#1913=VECTOR('',#7082,1.);
#1914=VECTOR('',#7083,1.);
#1915=VECTOR('',#7088,1.);
#1916=VECTOR('',#7089,1.);
#1917=VECTOR('',#7090,1.);
#1918=VECTOR('',#7091,1.);
#1919=VECTOR('',#7092,1.);
#1920=VECTOR('',#7093,1.);
#1921=VECTOR('',#7098,1.);
#1922=VECTOR('',#7099,1.);
#1923=VECTOR('',#7102,1.);
#1924=VECTOR('',#7105,1.);
#1925=VECTOR('',#7108,1.);
#1926=VECTOR('',#7111,1.);
#1927=VECTOR('',#7116,0.685);
#1928=VECTOR('',#7127,0.645);
#1929=VECTOR('',#7132,0.685);
#1930=VECTOR('',#7137,0.645);
#1931=VECTOR('',#7144,0.46);
#1932=VECTOR('',#7201,1.);
#1933=VECTOR('',#7202,1.);
#1934=VECTOR('',#7203,1.);
#1935=VECTOR('',#7204,1.);
#1936=VECTOR('',#7207,1.);
#1937=VECTOR('',#7208,1.);
#1938=VECTOR('',#7209,1.);
#1939=VECTOR('',#7212,1.);
#1940=VECTOR('',#7213,1.);
#1941=VECTOR('',#7214,1.);
#1942=VECTOR('',#7217,1.);
#1943=VECTOR('',#7218,1.);
#1944=VECTOR('',#7219,1.);
#1945=VECTOR('',#7222,1.);
#1946=VECTOR('',#7223,1.);
#1947=VECTOR('',#7224,1.);
#1948=VECTOR('',#7227,1.);
#1949=VECTOR('',#7228,1.);
#1950=VECTOR('',#7239,0.235);
#1951=VECTOR('',#7244,0.25);
#1952=VECTOR('',#7249,0.2125);
#1953=VECTOR('',#7256,1.);
#1954=VECTOR('',#7257,1.);
#1955=VECTOR('',#7258,1.);
#1956=VECTOR('',#7259,1.);
#1957=VECTOR('',#7260,1.);
#1958=VECTOR('',#7261,1.);
#1959=VECTOR('',#7262,1.);
#1960=VECTOR('',#7263,1.);
#1961=VECTOR('',#7266,1.);
#1962=VECTOR('',#7267,1.);
#1963=VECTOR('',#7268,1.);
#1964=VECTOR('',#7271,1.);
#1965=VECTOR('',#7272,1.);
#1966=VECTOR('',#7275,1.);
#1967=VECTOR('',#7276,1.);
#1968=VECTOR('',#7279,1.);
#1969=VECTOR('',#7280,1.);
#1970=VECTOR('',#7283,1.);
#1971=VECTOR('',#7284,1.);
#1972=VECTOR('',#7285,1.);
#1973=VECTOR('',#7286,1.);
#1974=VECTOR('',#7289,1.);
#1975=VECTOR('',#7292,1.);
#1976=VECTOR('',#7295,1.);
#1977=VECTOR('',#7308,0.4);
#1978=VECTOR('',#7313,0.425);
#1979=VECTOR('',#7318,0.41);
#1980=VECTOR('',#7327,0.26);
#1981=VECTOR('',#7332,0.25);
#1982=VECTOR('',#7337,0.225);
#1983=VECTOR('',#7342,1.);
#1984=VECTOR('',#7343,1.);
#1985=VECTOR('',#7344,1.);
#1986=VECTOR('',#7345,1.);
#1987=VECTOR('',#7348,1.);
#1988=VECTOR('',#7349,1.);
#1989=VECTOR('',#7350,1.);
#1990=VECTOR('',#7353,1.);
#1991=VECTOR('',#7354,1.);
#1992=VECTOR('',#7355,1.);
#1993=VECTOR('',#7358,1.);
#1994=VECTOR('',#7359,1.);
#1995=VECTOR('',#7360,1.);
#1996=VECTOR('',#7363,1.);
#1997=VECTOR('',#7364,1.);
#1998=VECTOR('',#7365,1.);
#1999=VECTOR('',#7368,1.);
#2000=VECTOR('',#7369,1.);
#2001=CIRCLE('',#5208,0.25);
#2002=CIRCLE('',#5209,0.25);
#2003=CIRCLE('',#5211,0.25);
#2004=CIRCLE('',#5212,0.25);
#2005=CIRCLE('',#5214,0.25);
#2006=CIRCLE('',#5215,0.25);
#2007=CIRCLE('',#5217,0.25);
#2008=CIRCLE('',#5218,0.25);
#2009=CIRCLE('',#5227,0.165);
#2010=CIRCLE('',#5228,0.165);
#2011=CIRCLE('',#5231,0.165);
#2012=CIRCLE('',#5232,0.165);
#2013=CIRCLE('',#5235,0.165);
#2014=CIRCLE('',#5236,0.165);
#2015=CIRCLE('',#5239,0.165);
#2016=CIRCLE('',#5240,0.165);
#2017=CIRCLE('',#5243,0.165);
#2018=CIRCLE('',#5244,0.165);
#2019=CIRCLE('',#5247,0.165);
#2020=CIRCLE('',#5248,0.165);
#2021=CIRCLE('',#5251,0.165);
#2022=CIRCLE('',#5252,0.165);
#2023=CIRCLE('',#5255,0.165);
#2024=CIRCLE('',#5256,0.165);
#2025=CIRCLE('',#5260,0.33);
#2026=CIRCLE('',#5261,0.33);
#2027=CIRCLE('',#5263,0.33);
#2028=CIRCLE('',#5264,0.33);
#2029=CIRCLE('',#5266,0.33);
#2030=CIRCLE('',#5267,0.33);
#2031=CIRCLE('',#5269,0.33);
#2032=CIRCLE('',#5270,0.33);
#2033=CIRCLE('',#5272,3.5);
#2034=CIRCLE('',#5274,3.5);
#2035=CIRCLE('',#5276,3.5);
#2036=CIRCLE('',#5278,3.5);
#2037=CIRCLE('',#5285,3.5);
#2038=CIRCLE('',#5287,3.5);
#2039=CIRCLE('',#5289,3.5);
#2040=CIRCLE('',#5291,3.5);
#2041=CIRCLE('',#5298,2.35);
#2042=CIRCLE('',#5299,2.35);
#2043=CIRCLE('',#5301,3.5);
#2044=CIRCLE('',#5302,3.5);
#2045=CIRCLE('',#5307,1.16);
#2046=CIRCLE('',#5308,1.16);
#2047=CIRCLE('',#5310,1.005);
#2048=CIRCLE('',#5312,1.005);
#2049=CIRCLE('',#5314,1.005);
#2050=CIRCLE('',#5316,1.005);
#2051=CIRCLE('',#5318,2.34);
#2052=CIRCLE('',#5319,2.34);
#2053=CIRCLE('',#5324,0.075);
#2054=CIRCLE('',#5325,1.);
#2055=CIRCLE('',#5328,1.16);
#2056=CIRCLE('',#5329,1.16);
#2057=CIRCLE('',#5331,1.005);
#2058=CIRCLE('',#5333,1.005);
#2059=CIRCLE('',#5335,1.005);
#2060=CIRCLE('',#5337,1.005);
#2061=CIRCLE('',#5339,2.34);
#2062=CIRCLE('',#5340,2.34);
#2063=CIRCLE('',#5345,0.075);
#2064=CIRCLE('',#5346,1.);
#2065=CIRCLE('',#5349,0.685);
#2066=CIRCLE('',#5351,0.685);
#2067=CIRCLE('',#5353,0.46);
#2068=CIRCLE('',#5355,2.34);
#2069=CIRCLE('',#5356,1.2);
#2070=CIRCLE('',#5358,2.34);
#2071=CIRCLE('',#5361,1.2);
#2072=CIRCLE('',#5365,0.225);
#2073=CIRCLE('',#5366,0.225);
#2074=CIRCLE('',#5368,0.225);
#2075=CIRCLE('',#5369,0.225);
#2076=CIRCLE('',#5371,0.225);
#2077=CIRCLE('',#5372,0.225);
#2078=CIRCLE('',#5374,0.225);
#2079=CIRCLE('',#5375,0.225);
#2080=CIRCLE('',#5377,2.34);
#2081=CIRCLE('',#5378,2.34);
#2082=CIRCLE('',#5380,1.8);
#2083=CIRCLE('',#5382,1.8);
#2084=CIRCLE('',#5384,3.5);
#2085=CIRCLE('',#5385,3.5);
#2086=CIRCLE('',#5390,0.225);
#2087=CIRCLE('',#5391,0.225);
#2088=CIRCLE('',#5393,0.225);
#2089=CIRCLE('',#5394,0.225);
#2090=CIRCLE('',#5396,0.225);
#2091=CIRCLE('',#5397,0.225);
#2092=CIRCLE('',#5399,0.225);
#2093=CIRCLE('',#5400,0.225);
#2094=CIRCLE('',#5402,2.34);
#2095=CIRCLE('',#5403,2.34);
#2096=CIRCLE('',#5405,1.8);
#2097=CIRCLE('',#5407,1.8);
#2098=CIRCLE('',#5409,3.5);
#2099=CIRCLE('',#5410,3.5);
#2100=CIRCLE('',#5430,1.63531);
#2101=CIRCLE('',#5431,1.63531);
#2102=CIRCLE('',#5432,0.412776);
#2103=CIRCLE('',#5433,1.63531);
#2104=CIRCLE('',#5434,1.63531);
#2105=CIRCLE('',#5436,1.63531);
#2106=CIRCLE('',#5438,1.);
#2107=CIRCLE('',#5439,1.);
#2108=CIRCLE('',#5441,1.1);
#2109=CIRCLE('',#5444,1.63531);
#2110=CIRCLE('',#5446,1.1);
#2111=CIRCLE('',#5450,1.71469);
#2112=CIRCLE('',#5451,1.71469);
#2113=CIRCLE('',#5452,0.412776);
#2114=CIRCLE('',#5453,1.71469);
#2115=CIRCLE('',#5454,1.71469);
#2116=CIRCLE('',#5456,1.71469);
#2117=CIRCLE('',#5458,2.25);
#2118=CIRCLE('',#5459,1.71469);
#2119=CIRCLE('',#5461,2.35);
#2120=CIRCLE('',#5463,2.35);
#2121=CIRCLE('',#5465,2.25);
#2122=CIRCLE('',#5470,0.3969);
#2123=CIRCLE('',#5472,0.3969);
#2124=CIRCLE('',#5474,0.3969);
#2125=CIRCLE('',#5476,0.3969);
#2126=CIRCLE('',#5478,0.3969);
#2127=CIRCLE('',#5480,0.3969);
#2128=CIRCLE('',#5482,0.3969);
#2129=CIRCLE('',#5484,0.3969);
#2130=CIRCLE('',#5487,0.405071403305639);
#2131=CIRCLE('',#5488,0.405071403305639);
#2132=CIRCLE('',#5490,1.706752);
#2133=CIRCLE('',#5491,1.706752);
#2134=CIRCLE('',#5492,1.706752);
#2135=CIRCLE('',#5493,1.706752);
#2136=CIRCLE('',#5494,1.706752);
#2137=CIRCLE('',#5495,1.706752);
#2138=CIRCLE('',#5496,1.706752);
#2139=CIRCLE('',#5497,1.706752);
#2140=CIRCLE('',#5498,1.706752);
#2141=CIRCLE('',#5500,1.643248);
#2142=CIRCLE('',#5501,0.405071403305639);
#2143=CIRCLE('',#5503,0.405071403305639);
#2144=CIRCLE('',#5505,1.643248);
#2145=CIRCLE('',#5506,0.405071403305639);
#2146=CIRCLE('',#5508,0.405071403305639);
#2147=CIRCLE('',#5510,1.643248);
#2148=CIRCLE('',#5511,0.405071403305639);
#2149=CIRCLE('',#5513,0.405071403305639);
#2150=CIRCLE('',#5515,1.643248);
#2151=CIRCLE('',#5516,0.405071403305639);
#2152=CIRCLE('',#5518,0.405071403305639);
#2153=CIRCLE('',#5520,1.643248);
#2154=CIRCLE('',#5521,0.405071403305639);
#2155=CIRCLE('',#5523,0.405071403305639);
#2156=CIRCLE('',#5525,1.643248);
#2157=CIRCLE('',#5526,0.405071403305639);
#2158=CIRCLE('',#5528,0.405071403305639);
#2159=CIRCLE('',#5530,1.643248);
#2160=CIRCLE('',#5531,1.643248);
#2161=CIRCLE('',#5532,1.643248);
#2162=CIRCLE('',#5534,0.405071403305639);
#2163=CIRCLE('',#5536,0.405071403305639);
#2164=CIRCLE('',#5541,1.70469);
#2165=CIRCLE('',#5542,1.65031);
#2166=CIRCLE('',#5544,1.70469);
#2167=CIRCLE('',#5546,1.65031);
#2168=CIRCLE('',#5549,1.70469);
#2169=CIRCLE('',#5550,1.65031);
#2170=CIRCLE('',#5552,1.70469);
#2171=CIRCLE('',#5554,1.65031);
#2172=CIRCLE('',#5563,0.45);
#2173=CIRCLE('',#5565,0.5);
#2174=CIRCLE('',#5567,0.5);
#2175=CIRCLE('',#5569,0.47);
#2176=CIRCLE('',#5571,0.32);
#2177=CIRCLE('',#5573,0.2942);
#2178=CIRCLE('',#5575,0.2942);
#2179=CIRCLE('',#5577,0.24);
#2180=CIRCLE('',#5589,0.3);
#2181=CIRCLE('',#5591,0.35);
#2182=CIRCLE('',#5593,0.35);
#2183=CIRCLE('',#5595,0.32);
#2184=CIRCLE('',#5597,0.22);
#2185=CIRCLE('',#5599,0.1954);
#2186=CIRCLE('',#5601,0.1954);
#2187=CIRCLE('',#5603,0.16);
#2188=CIRCLE('',#5616,0.21);
#2189=CIRCLE('',#5617,0.21);
#2190=CIRCLE('',#5621,1.);
#2191=CIRCLE('',#5625,1.);
#2192=CIRCLE('',#5626,1.);
#2193=CIRCLE('',#5627,1.);
#2194=CIRCLE('',#5629,1.2);
#2195=CIRCLE('',#5631,0.4);
#2196=CIRCLE('',#5633,1.2);
#2197=CIRCLE('',#5634,1.);
#2198=CIRCLE('',#5636,0.4);
#2199=CIRCLE('',#5639,0.4);
#2200=CIRCLE('',#5641,1.);
#2201=CIRCLE('',#5643,0.685);
#2202=CIRCLE('',#5644,0.685);
#2203=CIRCLE('',#5648,0.4);
#2204=CIRCLE('',#5654,1.005);
#2205=CIRCLE('',#5655,1.005);
#2206=CIRCLE('',#5657,1.35);
#2207=CIRCLE('',#5658,1.35);
#2208=CIRCLE('',#5663,0.21);
#2209=CIRCLE('',#5665,0.21);
#2210=CIRCLE('',#5666,0.21);
#2211=CIRCLE('',#5669,1.005);
#2212=CIRCLE('',#5670,1.005);
#2213=CIRCLE('',#5672,1.5);
#2214=CIRCLE('',#5673,1.5);
#2215=CIRCLE('',#5681,3.);
#2216=CIRCLE('',#5682,0.275);
#2217=CIRCLE('',#5683,0.275);
#2218=CIRCLE('',#5684,0.275);
#2219=CIRCLE('',#5685,0.275);
#2220=CIRCLE('',#5686,1.);
#2221=CIRCLE('',#5688,1.);
#2222=CIRCLE('',#5690,0.275);
#2223=CIRCLE('',#5692,0.275);
#2224=CIRCLE('',#5694,0.275);
#2225=CIRCLE('',#5696,0.275);
#2226=CIRCLE('',#5698,3.);
#2227=CIRCLE('',#5699,1.6);
#2228=CIRCLE('',#5702,1.6);
#2229=CIRCLE('',#5706,0.275);
#2230=CIRCLE('',#5707,0.275);
#2231=CIRCLE('',#5709,1.2);
#2232=CIRCLE('',#5710,1.2);
#2233=CIRCLE('',#5715,0.685);
#2234=CIRCLE('',#5717,0.685);
#2235=CIRCLE('',#5725,0.685);
#2236=CIRCLE('',#5727,0.605);
#2237=CIRCLE('',#5728,0.46);
#2238=CIRCLE('',#5731,0.685);
#2239=CIRCLE('',#5733,0.605);
#2240=CIRCLE('',#5735,0.46);
#2241=CIRCLE('',#5772,0.22);
#2242=CIRCLE('',#5774,0.24505);
#2243=CIRCLE('',#5776,0.24505);
#2244=CIRCLE('',#5778,0.175);
#2245=CIRCLE('',#5793,0.375);
#2246=CIRCLE('',#5795,0.425);
#2247=CIRCLE('',#5797,0.425);
#2248=CIRCLE('',#5799,0.395);
#2249=CIRCLE('',#5801,0.27);
#2250=CIRCLE('',#5803,0.24505);
#2251=CIRCLE('',#5805,0.24505);
#2252=CIRCLE('',#5807,0.2);
#2253=VERTEX_POINT('',#7400);
#2254=VERTEX_POINT('',#7402);
#2255=VERTEX_POINT('',#7406);
#2256=VERTEX_POINT('',#7408);
#2257=VERTEX_POINT('',#7412);
#2258=VERTEX_POINT('',#7414);
#2259=VERTEX_POINT('',#7418);
#2260=VERTEX_POINT('',#7420);
#2261=VERTEX_POINT('',#7424);
#2262=VERTEX_POINT('',#7425);
#2263=VERTEX_POINT('',#7427);
#2264=VERTEX_POINT('',#7429);
#2265=VERTEX_POINT('',#7433);
#2266=VERTEX_POINT('',#7435);
#2267=VERTEX_POINT('',#7439);
#2268=VERTEX_POINT('',#7441);
#2269=VERTEX_POINT('',#7451);
#2270=VERTEX_POINT('',#7453);
#2271=VERTEX_POINT('',#7458);
#2272=VERTEX_POINT('',#7460);
#2273=VERTEX_POINT('',#7465);
#2274=VERTEX_POINT('',#7467);
#2275=VERTEX_POINT('',#7472);
#2276=VERTEX_POINT('',#7474);
#2277=VERTEX_POINT('',#7479);
#2278=VERTEX_POINT('',#7481);
#2279=VERTEX_POINT('',#7486);
#2280=VERTEX_POINT('',#7488);
#2281=VERTEX_POINT('',#7493);
#2282=VERTEX_POINT('',#7495);
#2283=VERTEX_POINT('',#7500);
#2284=VERTEX_POINT('',#7502);
#2285=VERTEX_POINT('',#7507);
#2286=VERTEX_POINT('',#7508);
#2287=VERTEX_POINT('',#7545);
#2288=VERTEX_POINT('',#7547);
#2289=VERTEX_POINT('',#7585);
#2290=VERTEX_POINT('',#7587);
#2291=VERTEX_POINT('',#7591);
#2292=VERTEX_POINT('',#7593);
#2293=VERTEX_POINT('',#7597);
#2294=VERTEX_POINT('',#7599);
#2295=VERTEX_POINT('',#7603);
#2296=VERTEX_POINT('',#7605);
#2297=VERTEX_POINT('',#7609);
#2298=VERTEX_POINT('',#7610);
#2299=VERTEX_POINT('',#7612);
#2300=VERTEX_POINT('',#7614);
#2301=VERTEX_POINT('',#7618);
#2302=VERTEX_POINT('',#7620);
#2303=VERTEX_POINT('',#7622);
#2304=VERTEX_POINT('',#7626);
#2305=VERTEX_POINT('',#7627);
#2306=VERTEX_POINT('',#7629);
#2307=VERTEX_POINT('',#7631);
#2308=VERTEX_POINT('',#7635);
#2309=VERTEX_POINT('',#7637);
#2310=VERTEX_POINT('',#7639);
#2311=VERTEX_POINT('',#7654);
#2312=VERTEX_POINT('',#7655);
#2313=VERTEX_POINT('',#7657);
#2314=VERTEX_POINT('',#7659);
#2315=VERTEX_POINT('',#7663);
#2316=VERTEX_POINT('',#7665);
#2317=VERTEX_POINT('',#7667);
#2318=VERTEX_POINT('',#7671);
#2319=VERTEX_POINT('',#7672);
#2320=VERTEX_POINT('',#7674);
#2321=VERTEX_POINT('',#7676);
#2322=VERTEX_POINT('',#7680);
#2323=VERTEX_POINT('',#7682);
#2324=VERTEX_POINT('',#7684);
#2325=VERTEX_POINT('',#7699);
#2326=VERTEX_POINT('',#7701);
#2327=VERTEX_POINT('',#7705);
#2328=VERTEX_POINT('',#7707);
#2329=VERTEX_POINT('',#7714);
#2330=VERTEX_POINT('',#7716);
#2331=VERTEX_POINT('',#7720);
#2332=VERTEX_POINT('',#7723);
#2333=VERTEX_POINT('',#7726);
#2334=VERTEX_POINT('',#7730);
#2335=VERTEX_POINT('',#7734);
#2336=VERTEX_POINT('',#7736);
#2337=VERTEX_POINT('',#7743);
#2338=VERTEX_POINT('',#7748);
#2339=VERTEX_POINT('',#7750);
#2340=VERTEX_POINT('',#7754);
#2341=VERTEX_POINT('',#7757);
#2342=VERTEX_POINT('',#7760);
#2343=VERTEX_POINT('',#7764);
#2344=VERTEX_POINT('',#7768);
#2345=VERTEX_POINT('',#7770);
#2346=VERTEX_POINT('',#7777);
#2347=VERTEX_POINT('',#7782);
#2348=VERTEX_POINT('',#7783);
#2349=VERTEX_POINT('',#7785);
#2350=VERTEX_POINT('',#7801);
#2351=VERTEX_POINT('',#7805);
#2352=VERTEX_POINT('',#7806);
#2353=VERTEX_POINT('',#7808);
#2354=VERTEX_POINT('',#7810);
#2355=VERTEX_POINT('',#7829);
#2356=VERTEX_POINT('',#7833);
#2357=VERTEX_POINT('',#7838);
#2358=VERTEX_POINT('',#7839);
#2359=VERTEX_POINT('',#7878);
#2360=VERTEX_POINT('',#7884);
#2361=VERTEX_POINT('',#7886);
#2362=VERTEX_POINT('',#7890);
#2363=VERTEX_POINT('',#7892);
#2364=VERTEX_POINT('',#7896);
#2365=VERTEX_POINT('',#7898);
#2366=VERTEX_POINT('',#7902);
#2367=VERTEX_POINT('',#7904);
#2368=VERTEX_POINT('',#7908);
#2369=VERTEX_POINT('',#7910);
#2370=VERTEX_POINT('',#7914);
#2371=VERTEX_POINT('',#7917);
#2372=VERTEX_POINT('',#7921);
#2373=VERTEX_POINT('',#7923);
#2374=VERTEX_POINT('',#7930);
#2375=VERTEX_POINT('',#7932);
#2376=VERTEX_POINT('',#7936);
#2377=VERTEX_POINT('',#7938);
#2378=VERTEX_POINT('',#7942);
#2379=VERTEX_POINT('',#7944);
#2380=VERTEX_POINT('',#7948);
#2381=VERTEX_POINT('',#7950);
#2382=VERTEX_POINT('',#7954);
#2383=VERTEX_POINT('',#7956);
#2384=VERTEX_POINT('',#7960);
#2385=VERTEX_POINT('',#7963);
#2386=VERTEX_POINT('',#7967);
#2387=VERTEX_POINT('',#7969);
#2388=VERTEX_POINT('',#7976);
#2389=VERTEX_POINT('',#7977);
#2390=VERTEX_POINT('',#7979);
#2391=VERTEX_POINT('',#7981);
#2392=VERTEX_POINT('',#7985);
#2393=VERTEX_POINT('',#7987);
#2394=VERTEX_POINT('',#7991);
#2395=VERTEX_POINT('',#7993);
#2396=VERTEX_POINT('',#8003);
#2397=VERTEX_POINT('',#8004);
#2398=VERTEX_POINT('',#8006);
#2399=VERTEX_POINT('',#8008);
#2400=VERTEX_POINT('',#8012);
#2401=VERTEX_POINT('',#8014);
#2402=VERTEX_POINT('',#8018);
#2403=VERTEX_POINT('',#8020);
#2404=VERTEX_POINT('',#8031);
#2405=VERTEX_POINT('',#8032);
#2406=VERTEX_POINT('',#8035);
#2407=VERTEX_POINT('',#8037);
#2408=VERTEX_POINT('',#8041);
#2409=VERTEX_POINT('',#8045);
#2410=VERTEX_POINT('',#8047);
#2411=VERTEX_POINT('',#8051);
#2412=VERTEX_POINT('',#8056);
#2413=VERTEX_POINT('',#8060);
#2414=VERTEX_POINT('',#8066);
#2415=VERTEX_POINT('',#8067);
#2416=VERTEX_POINT('',#8070);
#2417=VERTEX_POINT('',#8072);
#2418=VERTEX_POINT('',#8076);
#2419=VERTEX_POINT('',#8080);
#2420=VERTEX_POINT('',#8082);
#2421=VERTEX_POINT('',#8085);
#2422=VERTEX_POINT('',#8089);
#2423=VERTEX_POINT('',#8093);
#2424=VERTEX_POINT('',#8101);
#2425=VERTEX_POINT('',#8102);
#2426=VERTEX_POINT('',#8105);
#2427=VERTEX_POINT('',#8106);
#2428=VERTEX_POINT('',#8109);
#2429=VERTEX_POINT('',#8110);
#2430=VERTEX_POINT('',#8113);
#2431=VERTEX_POINT('',#8114);
#2432=VERTEX_POINT('',#8117);
#2433=VERTEX_POINT('',#8118);
#2434=VERTEX_POINT('',#8121);
#2435=VERTEX_POINT('',#8122);
#2436=VERTEX_POINT('',#8125);
#2437=VERTEX_POINT('',#8126);
#2438=VERTEX_POINT('',#8129);
#2439=VERTEX_POINT('',#8130);
#2440=VERTEX_POINT('',#8134);
#2441=VERTEX_POINT('',#8135);
#2442=VERTEX_POINT('',#8158);
#2443=VERTEX_POINT('',#8160);
#2444=VERTEX_POINT('',#8185);
#2445=VERTEX_POINT('',#8187);
#2446=VERTEX_POINT('',#8210);
#2447=VERTEX_POINT('',#8212);
#2448=VERTEX_POINT('',#8235);
#2449=VERTEX_POINT('',#8237);
#2450=VERTEX_POINT('',#8250);
#2451=VERTEX_POINT('',#8253);
#2452=VERTEX_POINT('',#8266);
#2453=VERTEX_POINT('',#8268);
#2454=VERTEX_POINT('',#8291);
#2455=VERTEX_POINT('',#8293);
#2456=VERTEX_POINT('',#8316);
#2457=VERTEX_POINT('',#8318);
#2458=VERTEX_POINT('',#8341);
#2459=VERTEX_POINT('',#8343);
#2460=VERTEX_POINT('',#8368);
#2461=VERTEX_POINT('',#8372);
#2462=VERTEX_POINT('',#8397);
#2463=VERTEX_POINT('',#8401);
#2464=VERTEX_POINT('',#8426);
#2465=VERTEX_POINT('',#8430);
#2466=VERTEX_POINT('',#8431);
#2467=VERTEX_POINT('',#8458);
#2468=VERTEX_POINT('',#8462);
#2469=VERTEX_POINT('',#8487);
#2470=VERTEX_POINT('',#8491);
#2471=VERTEX_POINT('',#8516);
#2472=VERTEX_POINT('',#8520);
#2473=VERTEX_POINT('',#8545);
#2474=VERTEX_POINT('',#8548);
#2475=VERTEX_POINT('',#8550);
#2476=VERTEX_POINT('',#8582);
#2477=VERTEX_POINT('',#8584);
#2478=VERTEX_POINT('',#8587);
#2479=VERTEX_POINT('',#8591);
#2480=VERTEX_POINT('',#8596);
#2481=VERTEX_POINT('',#8598);
#2482=VERTEX_POINT('',#8601);
#2483=VERTEX_POINT('',#8605);
#2484=VERTEX_POINT('',#8616);
#2485=VERTEX_POINT('',#8619);
#2486=VERTEX_POINT('',#8623);
#2487=VERTEX_POINT('',#8627);
#2488=VERTEX_POINT('',#8631);
#2489=VERTEX_POINT('',#8634);
#2490=VERTEX_POINT('',#8638);
#2491=VERTEX_POINT('',#8642);
#2492=VERTEX_POINT('',#8647);
#2493=VERTEX_POINT('',#8648);
#2494=VERTEX_POINT('',#8650);
#2495=VERTEX_POINT('',#8652);
#2496=VERTEX_POINT('',#8656);
#2497=VERTEX_POINT('',#8658);
#2498=VERTEX_POINT('',#8662);
#2499=VERTEX_POINT('',#8664);
#2500=VERTEX_POINT('',#8668);
#2501=VERTEX_POINT('',#8670);
#2502=VERTEX_POINT('',#8674);
#2503=VERTEX_POINT('',#8676);
#2504=VERTEX_POINT('',#8686);
#2505=VERTEX_POINT('',#8689);
#2506=VERTEX_POINT('',#8693);
#2507=VERTEX_POINT('',#8697);
#2508=VERTEX_POINT('',#8701);
#2509=VERTEX_POINT('',#8704);
#2510=VERTEX_POINT('',#8708);
#2511=VERTEX_POINT('',#8712);
#2512=VERTEX_POINT('',#8717);
#2513=VERTEX_POINT('',#8718);
#2514=VERTEX_POINT('',#8720);
#2515=VERTEX_POINT('',#8722);
#2516=VERTEX_POINT('',#8726);
#2517=VERTEX_POINT('',#8728);
#2518=VERTEX_POINT('',#8732);
#2519=VERTEX_POINT('',#8734);
#2520=VERTEX_POINT('',#8738);
#2521=VERTEX_POINT('',#8740);
#2522=VERTEX_POINT('',#8744);
#2523=VERTEX_POINT('',#8746);
#2524=VERTEX_POINT('',#8757);
#2525=VERTEX_POINT('',#8759);
#2526=VERTEX_POINT('',#8764);
#2527=VERTEX_POINT('',#8765);
#2528=VERTEX_POINT('',#8767);
#2529=VERTEX_POINT('',#8769);
#2530=VERTEX_POINT('',#8773);
#2531=VERTEX_POINT('',#8775);
#2532=VERTEX_POINT('',#8779);
#2533=VERTEX_POINT('',#8781);
#2534=VERTEX_POINT('',#8787);
#2535=VERTEX_POINT('',#8789);
#2536=VERTEX_POINT('',#8793);
#2537=VERTEX_POINT('',#8794);
#2538=VERTEX_POINT('',#8832);
#2539=VERTEX_POINT('',#8835);
#2540=VERTEX_POINT('',#8838);
#2541=VERTEX_POINT('',#8840);
#2542=VERTEX_POINT('',#8843);
#2543=VERTEX_POINT('',#8848);
#2544=VERTEX_POINT('',#8852);
#2545=VERTEX_POINT('',#8856);
#2546=VERTEX_POINT('',#8858);
#2547=VERTEX_POINT('',#8863);
#2548=VERTEX_POINT('',#8864);
#2549=VERTEX_POINT('',#8911);
#2550=VERTEX_POINT('',#8919);
#2551=VERTEX_POINT('',#8921);
#2552=VERTEX_POINT('',#8925);
#2553=VERTEX_POINT('',#8927);
#2554=VERTEX_POINT('',#8934);
#2555=VERTEX_POINT('',#8935);
#2556=VERTEX_POINT('',#8939);
#2557=VERTEX_POINT('',#8954);
#2558=VERTEX_POINT('',#8956);
#2559=VERTEX_POINT('',#8958);
#2560=VERTEX_POINT('',#8995);
#2561=VERTEX_POINT('',#9014);
#2562=VERTEX_POINT('',#9016);
#2563=VERTEX_POINT('',#9020);
#2564=VERTEX_POINT('',#9022);
#2565=VERTEX_POINT('',#9029);
#2566=VERTEX_POINT('',#9030);
#2567=VERTEX_POINT('',#9032);
#2568=VERTEX_POINT('',#9034);
#2569=VERTEX_POINT('',#9038);
#2570=VERTEX_POINT('',#9040);
#2571=VERTEX_POINT('',#9044);
#2572=VERTEX_POINT('',#9046);
#2573=VERTEX_POINT('',#9050);
#2574=VERTEX_POINT('',#9052);
#2575=VERTEX_POINT('',#9054);
#2576=VERTEX_POINT('',#9056);
#2577=VERTEX_POINT('',#9058);
#2578=VERTEX_POINT('',#9064);
#2579=VERTEX_POINT('',#9068);
#2580=VERTEX_POINT('',#9072);
#2581=VERTEX_POINT('',#9076);
#2582=VERTEX_POINT('',#9080);
#2583=VERTEX_POINT('',#9082);
#2584=VERTEX_POINT('',#9087);
#2585=VERTEX_POINT('',#9093);
#2586=VERTEX_POINT('',#9095);
#2587=VERTEX_POINT('',#9099);
#2588=VERTEX_POINT('',#9101);
#2589=VERTEX_POINT('',#9108);
#2590=VERTEX_POINT('',#9109);
#2591=VERTEX_POINT('',#9111);
#2592=VERTEX_POINT('',#9113);
#2593=VERTEX_POINT('',#9115);
#2594=VERTEX_POINT('',#9117);
#2595=VERTEX_POINT('',#9120);
#2596=VERTEX_POINT('',#9123);
#2597=VERTEX_POINT('',#9124);
#2598=VERTEX_POINT('',#9126);
#2599=VERTEX_POINT('',#9128);
#2600=VERTEX_POINT('',#9130);
#2601=VERTEX_POINT('',#9132);
#2602=VERTEX_POINT('',#9135);
#2603=VERTEX_POINT('',#9150);
#2604=VERTEX_POINT('',#9154);
#2605=VERTEX_POINT('',#9156);
#2606=VERTEX_POINT('',#9161);
#2607=VERTEX_POINT('',#9165);
#2608=VERTEX_POINT('',#9169);
#2609=VERTEX_POINT('',#9201);
#2610=VERTEX_POINT('',#9202);
#2611=VERTEX_POINT('',#9204);
#2612=VERTEX_POINT('',#9206);
#2613=VERTEX_POINT('',#9210);
#2614=VERTEX_POINT('',#9212);
#2615=VERTEX_POINT('',#9216);
#2616=VERTEX_POINT('',#9218);
#2617=VERTEX_POINT('',#9222);
#2618=VERTEX_POINT('',#9224);
#2619=VERTEX_POINT('',#9228);
#2620=VERTEX_POINT('',#9230);
#2621=VERTEX_POINT('',#9238);
#2622=VERTEX_POINT('',#9241);
#2623=VERTEX_POINT('',#9245);
#2624=VERTEX_POINT('',#9249);
#2625=VERTEX_POINT('',#9255);
#2626=VERTEX_POINT('',#9256);
#2627=VERTEX_POINT('',#9258);
#2628=VERTEX_POINT('',#9260);
#2629=VERTEX_POINT('',#9262);
#2630=VERTEX_POINT('',#9264);
#2631=VERTEX_POINT('',#9266);
#2632=VERTEX_POINT('',#9268);
#2633=VERTEX_POINT('',#9272);
#2634=VERTEX_POINT('',#9274);
#2635=VERTEX_POINT('',#9278);
#2636=VERTEX_POINT('',#9282);
#2637=VERTEX_POINT('',#9286);
#2638=VERTEX_POINT('',#9290);
#2639=VERTEX_POINT('',#9291);
#2640=VERTEX_POINT('',#9294);
#2641=VERTEX_POINT('',#9306);
#2642=VERTEX_POINT('',#9309);
#2643=VERTEX_POINT('',#9313);
#2644=VERTEX_POINT('',#9317);
#2645=VERTEX_POINT('',#9321);
#2646=VERTEX_POINT('',#9324);
#2647=VERTEX_POINT('',#9328);
#2648=VERTEX_POINT('',#9332);
#2649=VERTEX_POINT('',#9337);
#2650=VERTEX_POINT('',#9338);
#2651=VERTEX_POINT('',#9340);
#2652=VERTEX_POINT('',#9342);
#2653=VERTEX_POINT('',#9346);
#2654=VERTEX_POINT('',#9348);
#2655=VERTEX_POINT('',#9352);
#2656=VERTEX_POINT('',#9354);
#2657=VERTEX_POINT('',#9358);
#2658=VERTEX_POINT('',#9360);
#2659=VERTEX_POINT('',#9364);
#2660=VERTEX_POINT('',#9366);
#2661=EDGE_CURVE('',#2253,#2253,#2001,.T.);
#2662=EDGE_CURVE('',#2253,#2254,#1361,.T.);
#2663=EDGE_CURVE('',#2254,#2254,#2002,.T.);
#2664=EDGE_CURVE('',#2255,#2255,#2003,.T.);
#2665=EDGE_CURVE('',#2255,#2256,#1362,.T.);
#2666=EDGE_CURVE('',#2256,#2256,#2004,.T.);
#2667=EDGE_CURVE('',#2257,#2257,#2005,.T.);
#2668=EDGE_CURVE('',#2257,#2258,#1363,.T.);
#2669=EDGE_CURVE('',#2258,#2258,#2006,.T.);
#2670=EDGE_CURVE('',#2259,#2259,#2007,.T.);
#2671=EDGE_CURVE('',#2259,#2260,#1364,.T.);
#2672=EDGE_CURVE('',#2260,#2260,#2008,.T.);
#2673=EDGE_CURVE('',#2261,#2262,#1365,.T.);
#2674=EDGE_CURVE('',#2262,#2263,#1366,.T.);
#2675=EDGE_CURVE('',#2264,#2263,#1367,.T.);
#2676=EDGE_CURVE('',#2261,#2264,#1368,.T.);
#2677=EDGE_CURVE('',#2265,#2261,#1369,.T.);
#2678=EDGE_CURVE('',#2266,#2264,#1370,.T.);
#2679=EDGE_CURVE('',#2265,#2266,#1371,.T.);
#2680=EDGE_CURVE('',#2267,#2265,#1372,.T.);
#2681=EDGE_CURVE('',#2268,#2266,#1373,.T.);
#2682=EDGE_CURVE('',#2267,#2268,#1374,.T.);
#2683=EDGE_CURVE('',#2262,#2267,#1375,.T.);
#2684=EDGE_CURVE('',#2263,#2268,#1376,.T.);
#2685=EDGE_CURVE('',#2269,#2269,#2009,.T.);
#2686=EDGE_CURVE('',#2269,#2270,#1377,.T.);
#2687=EDGE_CURVE('',#2270,#2270,#2010,.T.);
#2688=EDGE_CURVE('',#2271,#2271,#2011,.T.);
#2689=EDGE_CURVE('',#2271,#2272,#1378,.T.);
#2690=EDGE_CURVE('',#2272,#2272,#2012,.T.);
#2691=EDGE_CURVE('',#2273,#2273,#2013,.T.);
#2692=EDGE_CURVE('',#2273,#2274,#1379,.T.);
#2693=EDGE_CURVE('',#2274,#2274,#2014,.T.);
#2694=EDGE_CURVE('',#2275,#2275,#2015,.T.);
#2695=EDGE_CURVE('',#2275,#2276,#1380,.T.);
#2696=EDGE_CURVE('',#2276,#2276,#2016,.T.);
#2697=EDGE_CURVE('',#2277,#2277,#2017,.T.);
#2698=EDGE_CURVE('',#2277,#2278,#1381,.T.);
#2699=EDGE_CURVE('',#2278,#2278,#2018,.T.);
#2700=EDGE_CURVE('',#2279,#2279,#2019,.T.);
#2701=EDGE_CURVE('',#2279,#2280,#1382,.T.);
#2702=EDGE_CURVE('',#2280,#2280,#2020,.T.);
#2703=EDGE_CURVE('',#2281,#2281,#2021,.T.);
#2704=EDGE_CURVE('',#2281,#2282,#1383,.T.);
#2705=EDGE_CURVE('',#2282,#2282,#2022,.T.);
#2706=EDGE_CURVE('',#2283,#2283,#2023,.T.);
#2707=EDGE_CURVE('',#2283,#2284,#1384,.T.);
#2708=EDGE_CURVE('',#2284,#2284,#2024,.T.);
#2709=EDGE_CURVE('',#2285,#2286,#225,.T.);
#2710=EDGE_CURVE('',#2286,#2285,#226,.T.);
#2711=EDGE_CURVE('',#2286,#2287,#1385,.T.);
#2712=EDGE_CURVE('',#2288,#2287,#227,.T.);
#2713=EDGE_CURVE('',#2287,#2288,#228,.T.);
#2714=EDGE_CURVE('',#2289,#2289,#2025,.T.);
#2715=EDGE_CURVE('',#2289,#2290,#1386,.T.);
#2716=EDGE_CURVE('',#2290,#2290,#2026,.T.);
#2717=EDGE_CURVE('',#2291,#2291,#2027,.T.);
#2718=EDGE_CURVE('',#2291,#2292,#1387,.T.);
#2719=EDGE_CURVE('',#2292,#2292,#2028,.T.);
#2720=EDGE_CURVE('',#2293,#2293,#2029,.T.);
#2721=EDGE_CURVE('',#2293,#2294,#1388,.T.);
#2722=EDGE_CURVE('',#2294,#2294,#2030,.T.);
#2723=EDGE_CURVE('',#2295,#2295,#2031,.T.);
#2724=EDGE_CURVE('',#2295,#2296,#1389,.T.);
#2725=EDGE_CURVE('',#2296,#2296,#2032,.T.);
#2726=EDGE_CURVE('',#2297,#2298,#2033,.T.);
#2727=EDGE_CURVE('',#2297,#2299,#1390,.T.);
#2728=EDGE_CURVE('',#2299,#2300,#1391,.T.);
#2729=EDGE_CURVE('',#2300,#2298,#1392,.T.);
#2730=EDGE_CURVE('',#2298,#2301,#2034,.T.);
#2731=EDGE_CURVE('',#2298,#2302,#1393,.T.);
#2732=EDGE_CURVE('',#2302,#2303,#1394,.T.);
#2733=EDGE_CURVE('',#2303,#2301,#1395,.T.);
#2734=EDGE_CURVE('',#2304,#2305,#2035,.T.);
#2735=EDGE_CURVE('',#2304,#2306,#1396,.T.);
#2736=EDGE_CURVE('',#2306,#2307,#1397,.T.);
#2737=EDGE_CURVE('',#2307,#2305,#1398,.T.);
#2738=EDGE_CURVE('',#2308,#2304,#2036,.T.);
#2739=EDGE_CURVE('',#2308,#2309,#1399,.T.);
#2740=EDGE_CURVE('',#2309,#2310,#1400,.T.);
#2741=EDGE_CURVE('',#2310,#2304,#1401,.T.);
#2742=EDGE_CURVE('',#2305,#2297,#1402,.T.);
#2743=EDGE_CURVE('',#2307,#2299,#1403,.T.);
#2744=EDGE_CURVE('',#2301,#2308,#1404,.T.);
#2745=EDGE_CURVE('',#2309,#2303,#1405,.T.);
#2746=EDGE_CURVE('',#2310,#2302,#1406,.T.);
#2747=EDGE_CURVE('',#2306,#2300,#1407,.T.);
#2748=EDGE_CURVE('',#2311,#2312,#2037,.T.);
#2749=EDGE_CURVE('',#2311,#2313,#1408,.T.);
#2750=EDGE_CURVE('',#2313,#2314,#1409,.T.);
#2751=EDGE_CURVE('',#2314,#2312,#1410,.T.);
#2752=EDGE_CURVE('',#2312,#2315,#2038,.T.);
#2753=EDGE_CURVE('',#2312,#2316,#1411,.T.);
#2754=EDGE_CURVE('',#2316,#2317,#1412,.T.);
#2755=EDGE_CURVE('',#2317,#2315,#1413,.T.);
#2756=EDGE_CURVE('',#2318,#2319,#2039,.T.);
#2757=EDGE_CURVE('',#2318,#2320,#1414,.T.);
#2758=EDGE_CURVE('',#2320,#2321,#1415,.T.);
#2759=EDGE_CURVE('',#2321,#2319,#1416,.T.);
#2760=EDGE_CURVE('',#2322,#2318,#2040,.T.);
#2761=EDGE_CURVE('',#2322,#2323,#1417,.T.);
#2762=EDGE_CURVE('',#2323,#2324,#1418,.T.);
#2763=EDGE_CURVE('',#2324,#2318,#1419,.T.);
#2764=EDGE_CURVE('',#2319,#2311,#1420,.T.);
#2765=EDGE_CURVE('',#2321,#2313,#1421,.T.);
#2766=EDGE_CURVE('',#2315,#2322,#1422,.T.);
#2767=EDGE_CURVE('',#2323,#2317,#1423,.T.);
#2768=EDGE_CURVE('',#2324,#2316,#1424,.T.);
#2769=EDGE_CURVE('',#2320,#2314,#1425,.T.);
#2770=EDGE_CURVE('',#2325,#2325,#2041,.T.);
#2771=EDGE_CURVE('',#2325,#2326,#1426,.T.);
#2772=EDGE_CURVE('',#2326,#2326,#2042,.T.);
#2773=EDGE_CURVE('',#2327,#2327,#2043,.T.);
#2774=EDGE_CURVE('',#2327,#2328,#1427,.T.);
#2775=EDGE_CURVE('',#2328,#2328,#2044,.T.);
#2776=EDGE_CURVE('',#2329,#2329,#2045,.T.);
#2777=EDGE_CURVE('',#2329,#2330,#1428,.T.);
#2778=EDGE_CURVE('',#2330,#2330,#2046,.T.);
#2779=EDGE_CURVE('',#2331,#2331,#2047,.T.);
#2780=EDGE_CURVE('',#2332,#2332,#2048,.T.);
#2781=EDGE_CURVE('',#2332,#2333,#1429,.T.);
#2782=EDGE_CURVE('',#2333,#2333,#2049,.T.);
#2783=EDGE_CURVE('',#2334,#2334,#2050,.T.);
#2784=EDGE_CURVE('',#2334,#2331,#1430,.T.);
#2785=EDGE_CURVE('',#2335,#2335,#2051,.T.);
#2786=EDGE_CURVE('',#2335,#2336,#1431,.T.);
#2787=EDGE_CURVE('',#2336,#2336,#2052,.T.);
#2788=EDGE_CURVE('',#2337,#2337,#2053,.T.);
#2789=EDGE_CURVE('',#2337,#2337,#2054,.T.);
#2790=EDGE_CURVE('',#2338,#2338,#2055,.T.);
#2791=EDGE_CURVE('',#2338,#2339,#1432,.T.);
#2792=EDGE_CURVE('',#2339,#2339,#2056,.T.);
#2793=EDGE_CURVE('',#2340,#2340,#2057,.T.);
#2794=EDGE_CURVE('',#2341,#2341,#2058,.T.);
#2795=EDGE_CURVE('',#2341,#2342,#1433,.T.);
#2796=EDGE_CURVE('',#2342,#2342,#2059,.T.);
#2797=EDGE_CURVE('',#2343,#2343,#2060,.T.);
#2798=EDGE_CURVE('',#2343,#2340,#1434,.T.);
#2799=EDGE_CURVE('',#2344,#2344,#2061,.T.);
#2800=EDGE_CURVE('',#2344,#2345,#1435,.T.);
#2801=EDGE_CURVE('',#2345,#2345,#2062,.T.);
#2802=EDGE_CURVE('',#2346,#2346,#2063,.T.);
#2803=EDGE_CURVE('',#2346,#2346,#2064,.T.);
#2804=EDGE_CURVE('',#2347,#2348,#1436,.T.);
#2805=EDGE_CURVE('',#2349,#2347,#229,.T.);
#2806=EDGE_CURVE('',#2350,#2349,#1437,.T.);
#2807=EDGE_CURVE('',#2348,#2350,#2065,.T.);
#2808=EDGE_CURVE('',#2351,#2352,#1438,.T.);
#2809=EDGE_CURVE('',#2353,#2351,#2066,.T.);
#2810=EDGE_CURVE('',#2354,#2353,#1439,.T.);
#2811=EDGE_CURVE('',#2352,#2354,#230,.T.);
#2812=EDGE_CURVE('',#2348,#2351,#1440,.T.);
#2813=EDGE_CURVE('',#2353,#2350,#1441,.T.);
#2814=EDGE_CURVE('',#2355,#2355,#2067,.T.);
#2815=EDGE_CURVE('',#2349,#2354,#2068,.T.);
#2816=EDGE_CURVE('',#2356,#2356,#2069,.T.);
#2817=EDGE_CURVE('',#2347,#2352,#2070,.T.);
#2818=EDGE_CURVE('',#2357,#2358,#231,.T.);
#2819=EDGE_CURVE('',#2358,#2357,#232,.T.);
#2820=EDGE_CURVE('',#2358,#2355,#1442,.T.);
#2821=EDGE_CURVE('',#2356,#2359,#1443,.T.);
#2822=EDGE_CURVE('',#2359,#2359,#2071,.T.);
#2823=EDGE_CURVE('',#2360,#2360,#2072,.T.);
#2824=EDGE_CURVE('',#2360,#2361,#1444,.T.);
#2825=EDGE_CURVE('',#2361,#2361,#2073,.T.);
#2826=EDGE_CURVE('',#2362,#2362,#2074,.T.);
#2827=EDGE_CURVE('',#2362,#2363,#1445,.T.);
#2828=EDGE_CURVE('',#2363,#2363,#2075,.T.);
#2829=EDGE_CURVE('',#2364,#2364,#2076,.T.);
#2830=EDGE_CURVE('',#2364,#2365,#1446,.T.);
#2831=EDGE_CURVE('',#2365,#2365,#2077,.T.);
#2832=EDGE_CURVE('',#2366,#2366,#2078,.T.);
#2833=EDGE_CURVE('',#2366,#2367,#1447,.T.);
#2834=EDGE_CURVE('',#2367,#2367,#2079,.T.);
#2835=EDGE_CURVE('',#2368,#2368,#2080,.T.);
#2836=EDGE_CURVE('',#2368,#2369,#1448,.T.);
#2837=EDGE_CURVE('',#2369,#2369,#2081,.T.);
#2838=EDGE_CURVE('',#2370,#2370,#2082,.T.);
#2839=EDGE_CURVE('',#2370,#2371,#1449,.T.);
#2840=EDGE_CURVE('',#2371,#2371,#2083,.T.);
#2841=EDGE_CURVE('',#2372,#2372,#2084,.T.);
#2842=EDGE_CURVE('',#2372,#2373,#1450,.T.);
#2843=EDGE_CURVE('',#2373,#2373,#2085,.T.);
#2844=EDGE_CURVE('',#2374,#2374,#2086,.T.);
#2845=EDGE_CURVE('',#2374,#2375,#1451,.T.);
#2846=EDGE_CURVE('',#2375,#2375,#2087,.T.);
#2847=EDGE_CURVE('',#2376,#2376,#2088,.T.);
#2848=EDGE_CURVE('',#2376,#2377,#1452,.T.);
#2849=EDGE_CURVE('',#2377,#2377,#2089,.T.);
#2850=EDGE_CURVE('',#2378,#2378,#2090,.T.);
#2851=EDGE_CURVE('',#2378,#2379,#1453,.T.);
#2852=EDGE_CURVE('',#2379,#2379,#2091,.T.);
#2853=EDGE_CURVE('',#2380,#2380,#2092,.T.);
#2854=EDGE_CURVE('',#2380,#2381,#1454,.T.);
#2855=EDGE_CURVE('',#2381,#2381,#2093,.T.);
#2856=EDGE_CURVE('',#2382,#2382,#2094,.T.);
#2857=EDGE_CURVE('',#2382,#2383,#1455,.T.);
#2858=EDGE_CURVE('',#2383,#2383,#2095,.T.);
#2859=EDGE_CURVE('',#2384,#2384,#2096,.T.);
#2860=EDGE_CURVE('',#2385,#2385,#2097,.T.);
#2861=EDGE_CURVE('',#2385,#2384,#1456,.T.);
#2862=EDGE_CURVE('',#2386,#2386,#2098,.T.);
#2863=EDGE_CURVE('',#2386,#2387,#1457,.T.);
#2864=EDGE_CURVE('',#2387,#2387,#2099,.T.);
#2865=EDGE_CURVE('',#2388,#2389,#1458,.T.);
#2866=EDGE_CURVE('',#2389,#2390,#1459,.T.);
#2867=EDGE_CURVE('',#2391,#2390,#1460,.T.);
#2868=EDGE_CURVE('',#2388,#2391,#1461,.T.);
#2869=EDGE_CURVE('',#2392,#2388,#1462,.T.);
#2870=EDGE_CURVE('',#2393,#2391,#1463,.T.);
#2871=EDGE_CURVE('',#2392,#2393,#1464,.T.);
#2872=EDGE_CURVE('',#2394,#2392,#1465,.T.);
#2873=EDGE_CURVE('',#2395,#2393,#1466,.T.);
#2874=EDGE_CURVE('',#2394,#2395,#1467,.T.);
#2875=EDGE_CURVE('',#2389,#2394,#1468,.T.);
#2876=EDGE_CURVE('',#2390,#2395,#1469,.T.);
#2877=EDGE_CURVE('',#2396,#2397,#1470,.T.);
#2878=EDGE_CURVE('',#2397,#2398,#1471,.T.);
#2879=EDGE_CURVE('',#2399,#2398,#1472,.T.);
#2880=EDGE_CURVE('',#2396,#2399,#1473,.T.);
#2881=EDGE_CURVE('',#2400,#2396,#1474,.T.);
#2882=EDGE_CURVE('',#2401,#2399,#1475,.T.);
#2883=EDGE_CURVE('',#2400,#2401,#1476,.T.);
#2884=EDGE_CURVE('',#2402,#2400,#1477,.T.);
#2885=EDGE_CURVE('',#2403,#2401,#1478,.T.);
#2886=EDGE_CURVE('',#2402,#2403,#1479,.T.);
#2887=EDGE_CURVE('',#2397,#2402,#1480,.T.);
#2888=EDGE_CURVE('',#2398,#2403,#1481,.T.);
#2889=EDGE_CURVE('',#2404,#2405,#2100,.T.);
#2890=EDGE_CURVE('',#2405,#2404,#2101,.T.);
#2891=EDGE_CURVE('',#2405,#2406,#2102,.T.);
#2892=EDGE_CURVE('',#2407,#2406,#2103,.T.);
#2893=EDGE_CURVE('',#2406,#2407,#2104,.T.);
#2894=EDGE_CURVE('',#2407,#2408,#1482,.T.);
#2895=EDGE_CURVE('',#2408,#2408,#2105,.T.);
#2896=EDGE_CURVE('',#2409,#2409,#2106,.T.);
#2897=EDGE_CURVE('',#2409,#2410,#1483,.T.);
#2898=EDGE_CURVE('',#2410,#2410,#2107,.T.);
#2899=EDGE_CURVE('',#2410,#2411,#1484,.T.);
#2900=EDGE_CURVE('',#2411,#2411,#2108,.T.);
#2901=EDGE_CURVE('',#2412,#2412,#2109,.T.);
#2902=EDGE_CURVE('',#2412,#2404,#1485,.T.);
#2903=EDGE_CURVE('',#2413,#2413,#2110,.T.);
#2904=EDGE_CURVE('',#2413,#2409,#1486,.T.);
#2905=EDGE_CURVE('',#2414,#2415,#2111,.T.);
#2906=EDGE_CURVE('',#2415,#2414,#2112,.T.);
#2907=EDGE_CURVE('',#2415,#2416,#2113,.T.);
#2908=EDGE_CURVE('',#2417,#2416,#2114,.T.);
#2909=EDGE_CURVE('',#2416,#2417,#2115,.T.);
#2910=EDGE_CURVE('',#2418,#2418,#2116,.T.);
#2911=EDGE_CURVE('',#2418,#2417,#1487,.T.);
#2912=EDGE_CURVE('',#2419,#2419,#2117,.T.);
#2913=EDGE_CURVE('',#2420,#2420,#2118,.T.);
#2914=EDGE_CURVE('',#2421,#2421,#2119,.T.);
#2915=EDGE_CURVE('',#2421,#2419,#1488,.T.);
#2916=EDGE_CURVE('',#2422,#2422,#2120,.T.);
#2917=EDGE_CURVE('',#2422,#2421,#1489,.T.);
#2918=EDGE_CURVE('',#2423,#2423,#2121,.T.);
#2919=EDGE_CURVE('',#2423,#2422,#1490,.T.);
#2920=EDGE_CURVE('',#2414,#2420,#1491,.T.);
#2921=EDGE_CURVE('',#2424,#2425,#2122,.T.);
#2922=EDGE_CURVE('',#2426,#2427,#2123,.T.);
#2923=EDGE_CURVE('',#2428,#2429,#2124,.T.);
#2924=EDGE_CURVE('',#2430,#2431,#2125,.T.);
#2925=EDGE_CURVE('',#2432,#2433,#2126,.T.);
#2926=EDGE_CURVE('',#2434,#2435,#2127,.T.);
#2927=EDGE_CURVE('',#2436,#2437,#2128,.T.);
#2928=EDGE_CURVE('',#2438,#2439,#2129,.T.);
#2929=EDGE_CURVE('',#2440,#2441,#233,.T.);
#2930=EDGE_CURVE('',#2442,#2440,#2130,.T.);
#2931=EDGE_CURVE('',#2443,#2442,#234,.T.);
#2932=EDGE_CURVE('',#2441,#2443,#2131,.T.);
#2933=EDGE_CURVE('',#2444,#2442,#2132,.T.);
#2934=EDGE_CURVE('',#2444,#2445,#235,.T.);
#2935=EDGE_CURVE('',#2446,#2445,#2133,.T.);
#2936=EDGE_CURVE('',#2446,#2447,#236,.T.);
#2937=EDGE_CURVE('',#2448,#2447,#2134,.T.);
#2938=EDGE_CURVE('',#2448,#2449,#237,.T.);
#2939=EDGE_CURVE('',#2449,#2450,#1492,.T.);
#2940=EDGE_CURVE('',#2450,#2450,#2135,.T.);
#2941=EDGE_CURVE('',#2449,#2451,#238,.T.);
#2942=EDGE_CURVE('',#2452,#2451,#2136,.T.);
#2943=EDGE_CURVE('',#2452,#2453,#239,.T.);
#2944=EDGE_CURVE('',#2454,#2453,#2137,.T.);
#2945=EDGE_CURVE('',#2454,#2455,#240,.T.);
#2946=EDGE_CURVE('',#2456,#2455,#2138,.T.);
#2947=EDGE_CURVE('',#2456,#2457,#241,.T.);
#2948=EDGE_CURVE('',#2458,#2457,#2139,.T.);
#2949=EDGE_CURVE('',#2458,#2459,#242,.T.);
#2950=EDGE_CURVE('',#2443,#2459,#2140,.T.);
#2951=EDGE_CURVE('',#2440,#2460,#2141,.T.);
#2952=EDGE_CURVE('',#2460,#2444,#2142,.T.);
#2953=EDGE_CURVE('',#2461,#2460,#243,.T.);
#2954=EDGE_CURVE('',#2445,#2461,#2143,.T.);
#2955=EDGE_CURVE('',#2461,#2462,#2144,.T.);
#2956=EDGE_CURVE('',#2462,#2446,#2145,.T.);
#2957=EDGE_CURVE('',#2463,#2462,#244,.T.);
#2958=EDGE_CURVE('',#2447,#2463,#2146,.T.);
#2959=EDGE_CURVE('',#2463,#2464,#2147,.T.);
#2960=EDGE_CURVE('',#2464,#2448,#2148,.T.);
#2961=EDGE_CURVE('',#2465,#2466,#245,.T.);
#2962=EDGE_CURVE('',#2451,#2465,#2149,.T.);
#2963=EDGE_CURVE('',#2466,#2464,#246,.T.);
#2964=EDGE_CURVE('',#2465,#2467,#2150,.T.);
#2965=EDGE_CURVE('',#2467,#2452,#2151,.T.);
#2966=EDGE_CURVE('',#2468,#2467,#247,.T.);
#2967=EDGE_CURVE('',#2453,#2468,#2152,.T.);
#2968=EDGE_CURVE('',#2468,#2469,#2153,.T.);
#2969=EDGE_CURVE('',#2469,#2454,#2154,.T.);
#2970=EDGE_CURVE('',#2470,#2469,#248,.T.);
#2971=EDGE_CURVE('',#2455,#2470,#2155,.T.);
#2972=EDGE_CURVE('',#2470,#2471,#2156,.T.);
#2973=EDGE_CURVE('',#2471,#2456,#2157,.T.);
#2974=EDGE_CURVE('',#2472,#2471,#249,.T.);
#2975=EDGE_CURVE('',#2457,#2472,#2158,.T.);
#2976=EDGE_CURVE('',#2473,#2473,#2159,.T.);
#2977=EDGE_CURVE('',#2473,#2466,#1493,.T.);
#2978=EDGE_CURVE('',#2474,#2441,#2160,.T.);
#2979=EDGE_CURVE('',#2474,#2475,#250,.T.);
#2980=EDGE_CURVE('',#2472,#2475,#2161,.T.);
#2981=EDGE_CURVE('',#2459,#2474,#2162,.T.);
#2982=EDGE_CURVE('',#2475,#2458,#2163,.T.);
#2983=EDGE_CURVE('',#2476,#2476,#2164,.T.);
#2984=EDGE_CURVE('',#2477,#2477,#2165,.T.);
#2985=EDGE_CURVE('',#2478,#2478,#2166,.T.);
#2986=EDGE_CURVE('',#2478,#2476,#1494,.T.);
#2987=EDGE_CURVE('',#2479,#2479,#2167,.T.);
#2988=EDGE_CURVE('',#2479,#2477,#1495,.T.);
#2989=EDGE_CURVE('',#2480,#2480,#2168,.T.);
#2990=EDGE_CURVE('',#2481,#2481,#2169,.T.);
#2991=EDGE_CURVE('',#2482,#2482,#2170,.T.);
#2992=EDGE_CURVE('',#2482,#2480,#1496,.T.);
#2993=EDGE_CURVE('',#2483,#2483,#2171,.T.);
#2994=EDGE_CURVE('',#2483,#2481,#1497,.T.);
#2995=EDGE_CURVE('',#2484,#2484,#2172,.T.);
#2996=EDGE_CURVE('',#2485,#2485,#2173,.T.);
#2997=EDGE_CURVE('',#2485,#2484,#1498,.T.);
#2998=EDGE_CURVE('',#2486,#2486,#2174,.T.);
#2999=EDGE_CURVE('',#2486,#2485,#1499,.T.);
#3000=EDGE_CURVE('',#2487,#2487,#2175,.T.);
#3001=EDGE_CURVE('',#2487,#2486,#1500,.T.);
#3002=EDGE_CURVE('',#2488,#2488,#2176,.T.);
#3003=EDGE_CURVE('',#2489,#2489,#2177,.F.);
#3004=EDGE_CURVE('',#2489,#2488,#1501,.T.);
#3005=EDGE_CURVE('',#2490,#2490,#2178,.F.);
#3006=EDGE_CURVE('',#2490,#2489,#1502,.T.);
#3007=EDGE_CURVE('',#2491,#2491,#2179,.T.);
#3008=EDGE_CURVE('',#2491,#2490,#1503,.T.);
#3009=EDGE_CURVE('',#2492,#2493,#1504,.T.);
#3010=EDGE_CURVE('',#2493,#2494,#1505,.T.);
#3011=EDGE_CURVE('',#2494,#2495,#1506,.T.);
#3012=EDGE_CURVE('',#2492,#2495,#1507,.T.);
#3013=EDGE_CURVE('',#2493,#2496,#1508,.T.);
#3014=EDGE_CURVE('',#2496,#2497,#1509,.T.);
#3015=EDGE_CURVE('',#2497,#2494,#1510,.T.);
#3016=EDGE_CURVE('',#2496,#2498,#1511,.T.);
#3017=EDGE_CURVE('',#2498,#2499,#1512,.T.);
#3018=EDGE_CURVE('',#2499,#2497,#1513,.T.);
#3019=EDGE_CURVE('',#2498,#2500,#1514,.T.);
#3020=EDGE_CURVE('',#2500,#2501,#1515,.T.);
#3021=EDGE_CURVE('',#2501,#2499,#1516,.T.);
#3022=EDGE_CURVE('',#2500,#2502,#1517,.T.);
#3023=EDGE_CURVE('',#2502,#2503,#1518,.T.);
#3024=EDGE_CURVE('',#2503,#2501,#1519,.T.);
#3025=EDGE_CURVE('',#2502,#2492,#1520,.T.);
#3026=EDGE_CURVE('',#2495,#2503,#1521,.T.);
#3027=EDGE_CURVE('',#2504,#2504,#2180,.T.);
#3028=EDGE_CURVE('',#2505,#2505,#2181,.T.);
#3029=EDGE_CURVE('',#2505,#2504,#1522,.T.);
#3030=EDGE_CURVE('',#2506,#2506,#2182,.T.);
#3031=EDGE_CURVE('',#2506,#2505,#1523,.T.);
#3032=EDGE_CURVE('',#2507,#2507,#2183,.T.);
#3033=EDGE_CURVE('',#2507,#2506,#1524,.T.);
#3034=EDGE_CURVE('',#2508,#2508,#2184,.T.);
#3035=EDGE_CURVE('',#2509,#2509,#2185,.F.);
#3036=EDGE_CURVE('',#2509,#2508,#1525,.T.);
#3037=EDGE_CURVE('',#2510,#2510,#2186,.F.);
#3038=EDGE_CURVE('',#2510,#2509,#1526,.T.);
#3039=EDGE_CURVE('',#2511,#2511,#2187,.T.);
#3040=EDGE_CURVE('',#2511,#2510,#1527,.T.);
#3041=EDGE_CURVE('',#2512,#2513,#1528,.T.);
#3042=EDGE_CURVE('',#2513,#2514,#1529,.T.);
#3043=EDGE_CURVE('',#2514,#2515,#1530,.T.);
#3044=EDGE_CURVE('',#2512,#2515,#1531,.T.);
#3045=EDGE_CURVE('',#2513,#2516,#1532,.T.);
#3046=EDGE_CURVE('',#2516,#2517,#1533,.T.);
#3047=EDGE_CURVE('',#2517,#2514,#1534,.T.);
#3048=EDGE_CURVE('',#2516,#2518,#1535,.T.);
#3049=EDGE_CURVE('',#2518,#2519,#1536,.T.);
#3050=EDGE_CURVE('',#2519,#2517,#1537,.T.);
#3051=EDGE_CURVE('',#2518,#2520,#1538,.T.);
#3052=EDGE_CURVE('',#2520,#2521,#1539,.T.);
#3053=EDGE_CURVE('',#2521,#2519,#1540,.T.);
#3054=EDGE_CURVE('',#2520,#2522,#1541,.T.);
#3055=EDGE_CURVE('',#2522,#2523,#1542,.T.);
#3056=EDGE_CURVE('',#2523,#2521,#1543,.T.);
#3057=EDGE_CURVE('',#2522,#2512,#1544,.T.);
#3058=EDGE_CURVE('',#2515,#2523,#1545,.T.);
#3059=EDGE_CURVE('',#2524,#2524,#2188,.T.);
#3060=EDGE_CURVE('',#2524,#2525,#1546,.T.);
#3061=EDGE_CURVE('',#2525,#2525,#2189,.T.);
#3062=EDGE_CURVE('',#2526,#2527,#1547,.T.);
#3063=EDGE_CURVE('',#2528,#2526,#1548,.T.);
#3064=EDGE_CURVE('',#2529,#2528,#1549,.T.);
#3065=EDGE_CURVE('',#2529,#2527,#1550,.T.);
#3066=EDGE_CURVE('',#2527,#2530,#2190,.T.);
#3067=EDGE_CURVE('',#2531,#2529,#1551,.T.);
#3068=EDGE_CURVE('',#2530,#2531,#1552,.T.);
#3069=EDGE_CURVE('',#2530,#2532,#1553,.T.);
#3070=EDGE_CURVE('',#2531,#2533,#1554,.T.);
#3071=EDGE_CURVE('',#2532,#2533,#1555,.T.);
#3072=EDGE_CURVE('',#2533,#2528,#1556,.T.);
#3073=EDGE_CURVE('',#2534,#2532,#2191,.T.);
#3074=EDGE_CURVE('',#2534,#2535,#1557,.T.);
#3075=EDGE_CURVE('',#2535,#2535,#2192,.T.);
#3076=EDGE_CURVE('',#2526,#2534,#2193,.T.);
#3077=EDGE_CURVE('',#2536,#2537,#251,.T.);
#3078=EDGE_CURVE('',#2537,#2536,#252,.T.);
#3079=EDGE_CURVE('',#2538,#2538,#2194,.T.);
#3080=EDGE_CURVE('',#2539,#2539,#2195,.T.);
#3081=EDGE_CURVE('',#2540,#2540,#2196,.T.);
#3082=EDGE_CURVE('',#2541,#2541,#2197,.T.);
#3083=EDGE_CURVE('',#2542,#2542,#2198,.T.);
#3084=EDGE_CURVE('',#2538,#2540,#1558,.T.);
#3085=EDGE_CURVE('',#2543,#2543,#2199,.T.);
#3086=EDGE_CURVE('',#2543,#2542,#1559,.T.);
#3087=EDGE_CURVE('',#2541,#2544,#1560,.T.);
#3088=EDGE_CURVE('',#2544,#2544,#2200,.T.);
#3089=EDGE_CURVE('',#2545,#2545,#2201,.T.);
#3090=EDGE_CURVE('',#2545,#2546,#1561,.T.);
#3091=EDGE_CURVE('',#2546,#2546,#2202,.T.);
#3092=EDGE_CURVE('',#2547,#2548,#253,.T.);
#3093=EDGE_CURVE('',#2548,#2547,#254,.T.);
#3094=EDGE_CURVE('',#2548,#2537,#1562,.T.);
#3095=EDGE_CURVE('',#2539,#2549,#1563,.T.);
#3096=EDGE_CURVE('',#2549,#2549,#2203,.T.);
#3097=EDGE_CURVE('',#2550,#2550,#2204,.T.);
#3098=EDGE_CURVE('',#2550,#2551,#1564,.T.);
#3099=EDGE_CURVE('',#2551,#2551,#2205,.T.);
#3100=EDGE_CURVE('',#2552,#2552,#2206,.T.);
#3101=EDGE_CURVE('',#2552,#2553,#1565,.T.);
#3102=EDGE_CURVE('',#2553,#2553,#2207,.T.);
#3103=EDGE_CURVE('',#2554,#2555,#1566,.T.);
#3104=EDGE_CURVE('',#2554,#2555,#2208,.T.);
#3105=EDGE_CURVE('',#2556,#2554,#255,.T.);
#3106=EDGE_CURVE('',#2557,#2556,#2209,.T.);
#3107=EDGE_CURVE('',#2557,#2558,#1567,.T.);
#3108=EDGE_CURVE('',#2559,#2558,#256,.T.);
#3109=EDGE_CURVE('',#2558,#2559,#257,.T.);
#3110=EDGE_CURVE('',#2560,#2557,#2210,.T.);
#3111=EDGE_CURVE('',#2555,#2560,#258,.T.);
#3112=EDGE_CURVE('',#2560,#2556,#1568,.T.);
#3113=EDGE_CURVE('',#2561,#2561,#2211,.T.);
#3114=EDGE_CURVE('',#2561,#2562,#1569,.T.);
#3115=EDGE_CURVE('',#2562,#2562,#2212,.T.);
#3116=EDGE_CURVE('',#2563,#2563,#2213,.T.);
#3117=EDGE_CURVE('',#2563,#2564,#1570,.T.);
#3118=EDGE_CURVE('',#2564,#2564,#2214,.T.);
#3119=EDGE_CURVE('',#2565,#2566,#1571,.T.);
#3120=EDGE_CURVE('',#2565,#2567,#1572,.T.);
#3121=EDGE_CURVE('',#2568,#2567,#1573,.T.);
#3122=EDGE_CURVE('',#2566,#2568,#1574,.T.);
#3123=EDGE_CURVE('',#2569,#2565,#1575,.T.);
#3124=EDGE_CURVE('',#2569,#2570,#1576,.T.);
#3125=EDGE_CURVE('',#2567,#2570,#1577,.T.);
#3126=EDGE_CURVE('',#2571,#2569,#1578,.T.);
#3127=EDGE_CURVE('',#2572,#2571,#1579,.T.);
#3128=EDGE_CURVE('',#2570,#2572,#1580,.T.);
#3129=EDGE_CURVE('',#2573,#2573,#2215,.T.);
#3130=EDGE_CURVE('',#2574,#2574,#2216,.T.);
#3131=EDGE_CURVE('',#2575,#2575,#2217,.T.);
#3132=EDGE_CURVE('',#2576,#2576,#2218,.T.);
#3133=EDGE_CURVE('',#2577,#2577,#2219,.T.);
#3134=EDGE_CURVE('',#2572,#2568,#2220,.T.);
#3135=EDGE_CURVE('',#2571,#2566,#2221,.T.);
#3136=EDGE_CURVE('',#2578,#2578,#2222,.T.);
#3137=EDGE_CURVE('',#2578,#2574,#1581,.T.);
#3138=EDGE_CURVE('',#2579,#2579,#2223,.T.);
#3139=EDGE_CURVE('',#2579,#2575,#1582,.T.);
#3140=EDGE_CURVE('',#2580,#2580,#2224,.T.);
#3141=EDGE_CURVE('',#2580,#2576,#1583,.T.);
#3142=EDGE_CURVE('',#2581,#2581,#2225,.T.);
#3143=EDGE_CURVE('',#2581,#2577,#1584,.T.);
#3144=EDGE_CURVE('',#2582,#2582,#2226,.T.);
#3145=EDGE_CURVE('',#2583,#2583,#2227,.T.);
#3146=EDGE_CURVE('',#2573,#2582,#1585,.T.);
#3147=EDGE_CURVE('',#2583,#2584,#1586,.T.);
#3148=EDGE_CURVE('',#2584,#2584,#2228,.T.);
#3149=EDGE_CURVE('',#2585,#2585,#2229,.T.);
#3150=EDGE_CURVE('',#2585,#2586,#1587,.T.);
#3151=EDGE_CURVE('',#2586,#2586,#2230,.T.);
#3152=EDGE_CURVE('',#2587,#2587,#2231,.T.);
#3153=EDGE_CURVE('',#2587,#2588,#1588,.T.);
#3154=EDGE_CURVE('',#2588,#2588,#2232,.T.);
#3155=EDGE_CURVE('',#2589,#2590,#1589,.T.);
#3156=EDGE_CURVE('',#2590,#2591,#1590,.T.);
#3157=EDGE_CURVE('',#2591,#2592,#1591,.T.);
#3158=EDGE_CURVE('',#2592,#2593,#1592,.T.);
#3159=EDGE_CURVE('',#2593,#2594,#1593,.T.);
#3160=EDGE_CURVE('',#2594,#2589,#1594,.T.);
#3161=EDGE_CURVE('',#2595,#2595,#2233,.T.);
#3162=EDGE_CURVE('',#2596,#2597,#1595,.T.);
#3163=EDGE_CURVE('',#2597,#2598,#1596,.T.);
#3164=EDGE_CURVE('',#2598,#2599,#1597,.T.);
#3165=EDGE_CURVE('',#2599,#2600,#1598,.T.);
#3166=EDGE_CURVE('',#2600,#2601,#1599,.T.);
#3167=EDGE_CURVE('',#2601,#2596,#1600,.T.);
#3168=EDGE_CURVE('',#2602,#2602,#2234,.T.);
#3169=EDGE_CURVE('',#2596,#2590,#1601,.T.);
#3170=EDGE_CURVE('',#2591,#2601,#1602,.T.);
#3171=EDGE_CURVE('',#2592,#2600,#1603,.T.);
#3172=EDGE_CURVE('',#2593,#2599,#1604,.T.);
#3173=EDGE_CURVE('',#2594,#2598,#1605,.T.);
#3174=EDGE_CURVE('',#2589,#2597,#1606,.T.);
#3175=EDGE_CURVE('',#2602,#2603,#1607,.T.);
#3176=EDGE_CURVE('',#2603,#2603,#2235,.T.);
#3177=EDGE_CURVE('',#2604,#2604,#2236,.T.);
#3178=EDGE_CURVE('',#2605,#2605,#2237,.T.);
#3179=EDGE_CURVE('',#2603,#2604,#1608,.T.);
#3180=EDGE_CURVE('',#2606,#2606,#2238,.T.);
#3181=EDGE_CURVE('',#2606,#2595,#1609,.T.);
#3182=EDGE_CURVE('',#2607,#2607,#2239,.T.);
#3183=EDGE_CURVE('',#2607,#2606,#1610,.T.);
#3184=EDGE_CURVE('',#2608,#2608,#2240,.T.);
#3185=EDGE_CURVE('',#2608,#2605,#1611,.T.);
#3186=EDGE_CURVE('',#2609,#2610,#1612,.T.);
#3187=EDGE_CURVE('',#2609,#2611,#1613,.T.);
#3188=EDGE_CURVE('',#2611,#2612,#1614,.T.);
#3189=EDGE_CURVE('',#2610,#2612,#1615,.T.);
#3190=EDGE_CURVE('',#2613,#2609,#1616,.T.);
#3191=EDGE_CURVE('',#2613,#2614,#1617,.T.);
#3192=EDGE_CURVE('',#2614,#2611,#1618,.T.);
#3193=EDGE_CURVE('',#2615,#2613,#1619,.T.);
#3194=EDGE_CURVE('',#2615,#2616,#1620,.T.);
#3195=EDGE_CURVE('',#2616,#2614,#1621,.T.);
#3196=EDGE_CURVE('',#2617,#2615,#1622,.T.);
#3197=EDGE_CURVE('',#2617,#2618,#1623,.T.);
#3198=EDGE_CURVE('',#2618,#2616,#1624,.T.);
#3199=EDGE_CURVE('',#2619,#2617,#1625,.T.);
#3200=EDGE_CURVE('',#2619,#2620,#1626,.T.);
#3201=EDGE_CURVE('',#2620,#2618,#1627,.T.);
#3202=EDGE_CURVE('',#2610,#2619,#1628,.T.);
#3203=EDGE_CURVE('',#2612,#2620,#1629,.T.);
#3204=EDGE_CURVE('',#2621,#2621,#2241,.T.);
#3205=EDGE_CURVE('',#2622,#2622,#2242,.T.);
#3206=EDGE_CURVE('',#2622,#2621,#1630,.T.);
#3207=EDGE_CURVE('',#2623,#2623,#2243,.F.);
#3208=EDGE_CURVE('',#2623,#2622,#1631,.T.);
#3209=EDGE_CURVE('',#2624,#2624,#2244,.T.);
#3210=EDGE_CURVE('',#2624,#2623,#1632,.T.);
#3211=EDGE_CURVE('',#2625,#2626,#1633,.T.);
#3212=EDGE_CURVE('',#2627,#2625,#1634,.T.);
#3213=EDGE_CURVE('',#2628,#2627,#1635,.T.);
#3214=EDGE_CURVE('',#2629,#2628,#1636,.T.);
#3215=EDGE_CURVE('',#2630,#2629,#1637,.T.);
#3216=EDGE_CURVE('',#2631,#2630,#1638,.T.);
#3217=EDGE_CURVE('',#2632,#2631,#1639,.T.);
#3218=EDGE_CURVE('',#2626,#2632,#1640,.T.);
#3219=EDGE_CURVE('',#2629,#2633,#1641,.T.);
#3220=EDGE_CURVE('',#2633,#2634,#1642,.T.);
#3221=EDGE_CURVE('',#2634,#2630,#1643,.T.);
#3222=EDGE_CURVE('',#2635,#2628,#1644,.T.);
#3223=EDGE_CURVE('',#2635,#2633,#1645,.T.);
#3224=EDGE_CURVE('',#2627,#2636,#1646,.T.);
#3225=EDGE_CURVE('',#2636,#2635,#1647,.T.);
#3226=EDGE_CURVE('',#2637,#2625,#1648,.T.);
#3227=EDGE_CURVE('',#2637,#2636,#1649,.T.);
#3228=EDGE_CURVE('',#2638,#2639,#1650,.T.);
#3229=EDGE_CURVE('',#2634,#2638,#1651,.T.);
#3230=EDGE_CURVE('',#2640,#2637,#1652,.T.);
#3231=EDGE_CURVE('',#2639,#2640,#1653,.T.);
#3232=EDGE_CURVE('',#2631,#2638,#1654,.T.);
#3233=EDGE_CURVE('',#2626,#2640,#1655,.T.);
#3234=EDGE_CURVE('',#2639,#2632,#1656,.T.);
#3235=EDGE_CURVE('',#2641,#2641,#2245,.T.);
#3236=EDGE_CURVE('',#2642,#2642,#2246,.T.);
#3237=EDGE_CURVE('',#2642,#2641,#1657,.T.);
#3238=EDGE_CURVE('',#2643,#2643,#2247,.T.);
#3239=EDGE_CURVE('',#2643,#2642,#1658,.T.);
#3240=EDGE_CURVE('',#2644,#2644,#2248,.T.);
#3241=EDGE_CURVE('',#2644,#2643,#1659,.T.);
#3242=EDGE_CURVE('',#2645,#2645,#2249,.T.);
#3243=EDGE_CURVE('',#2646,#2646,#2250,.F.);
#3244=EDGE_CURVE('',#2646,#2645,#1660,.T.);
#3245=EDGE_CURVE('',#2647,#2647,#2251,.F.);
#3246=EDGE_CURVE('',#2647,#2646,#1661,.T.);
#3247=EDGE_CURVE('',#2648,#2648,#2252,.T.);
#3248=EDGE_CURVE('',#2648,#2647,#1662,.T.);
#3249=EDGE_CURVE('',#2649,#2650,#1663,.T.);
#3250=EDGE_CURVE('',#2650,#2651,#1664,.T.);
#3251=EDGE_CURVE('',#2651,#2652,#1665,.T.);
#3252=EDGE_CURVE('',#2649,#2652,#1666,.T.);
#3253=EDGE_CURVE('',#2650,#2653,#1667,.T.);
#3254=EDGE_CURVE('',#2653,#2654,#1668,.T.);
#3255=EDGE_CURVE('',#2654,#2651,#1669,.T.);
#3256=EDGE_CURVE('',#2653,#2655,#1670,.T.);
#3257=EDGE_CURVE('',#2655,#2656,#1671,.T.);
#3258=EDGE_CURVE('',#2656,#2654,#1672,.T.);
#3259=EDGE_CURVE('',#2655,#2657,#1673,.T.);
#3260=EDGE_CURVE('',#2657,#2658,#1674,.T.);
#3261=EDGE_CURVE('',#2658,#2656,#1675,.T.);
#3262=EDGE_CURVE('',#2657,#2659,#1676,.T.);
#3263=EDGE_CURVE('',#2659,#2660,#1677,.T.);
#3264=EDGE_CURVE('',#2660,#2658,#1678,.T.);
#3265=EDGE_CURVE('',#2659,#2649,#1679,.T.);
#3266=EDGE_CURVE('',#2652,#2660,#1680,.T.);
#3267=ORIENTED_EDGE('',*,*,#2661,.F.);
#3268=ORIENTED_EDGE('',*,*,#2662,.T.);
#3269=ORIENTED_EDGE('',*,*,#2663,.F.);
#3270=ORIENTED_EDGE('',*,*,#2662,.F.);
#3271=ORIENTED_EDGE('',*,*,#2664,.F.);
#3272=ORIENTED_EDGE('',*,*,#2665,.T.);
#3273=ORIENTED_EDGE('',*,*,#2666,.F.);
#3274=ORIENTED_EDGE('',*,*,#2665,.F.);
#3275=ORIENTED_EDGE('',*,*,#2667,.F.);
#3276=ORIENTED_EDGE('',*,*,#2668,.T.);
#3277=ORIENTED_EDGE('',*,*,#2669,.F.);
#3278=ORIENTED_EDGE('',*,*,#2668,.F.);
#3279=ORIENTED_EDGE('',*,*,#2670,.F.);
#3280=ORIENTED_EDGE('',*,*,#2671,.T.);
#3281=ORIENTED_EDGE('',*,*,#2672,.F.);
#3282=ORIENTED_EDGE('',*,*,#2671,.F.);
#3283=ORIENTED_EDGE('',*,*,#2673,.T.);
#3284=ORIENTED_EDGE('',*,*,#2674,.T.);
#3285=ORIENTED_EDGE('',*,*,#2675,.F.);
#3286=ORIENTED_EDGE('',*,*,#2676,.F.);
#3287=ORIENTED_EDGE('',*,*,#2677,.T.);
#3288=ORIENTED_EDGE('',*,*,#2676,.T.);
#3289=ORIENTED_EDGE('',*,*,#2678,.F.);
#3290=ORIENTED_EDGE('',*,*,#2679,.F.);
#3291=ORIENTED_EDGE('',*,*,#2680,.T.);
#3292=ORIENTED_EDGE('',*,*,#2679,.T.);
#3293=ORIENTED_EDGE('',*,*,#2681,.F.);
#3294=ORIENTED_EDGE('',*,*,#2682,.F.);
#3295=ORIENTED_EDGE('',*,*,#2683,.T.);
#3296=ORIENTED_EDGE('',*,*,#2682,.T.);
#3297=ORIENTED_EDGE('',*,*,#2684,.F.);
#3298=ORIENTED_EDGE('',*,*,#2674,.F.);
#3299=ORIENTED_EDGE('',*,*,#2684,.T.);
#3300=ORIENTED_EDGE('',*,*,#2681,.T.);
#3301=ORIENTED_EDGE('',*,*,#2678,.T.);
#3302=ORIENTED_EDGE('',*,*,#2675,.T.);
#3303=ORIENTED_EDGE('',*,*,#2663,.T.);
#3304=ORIENTED_EDGE('',*,*,#2666,.T.);
#3305=ORIENTED_EDGE('',*,*,#2669,.T.);
#3306=ORIENTED_EDGE('',*,*,#2672,.T.);
#3307=ORIENTED_EDGE('',*,*,#2683,.F.);
#3308=ORIENTED_EDGE('',*,*,#2673,.F.);
#3309=ORIENTED_EDGE('',*,*,#2677,.F.);
#3310=ORIENTED_EDGE('',*,*,#2680,.F.);
#3311=ORIENTED_EDGE('',*,*,#2661,.T.);
#3312=ORIENTED_EDGE('',*,*,#2664,.T.);
#3313=ORIENTED_EDGE('',*,*,#2667,.T.);
#3314=ORIENTED_EDGE('',*,*,#2670,.T.);
#3315=ORIENTED_EDGE('',*,*,#2685,.F.);
#3316=ORIENTED_EDGE('',*,*,#2686,.T.);
#3317=ORIENTED_EDGE('',*,*,#2687,.F.);
#3318=ORIENTED_EDGE('',*,*,#2686,.F.);
#3319=ORIENTED_EDGE('',*,*,#2685,.T.);
#3320=ORIENTED_EDGE('',*,*,#2688,.F.);
#3321=ORIENTED_EDGE('',*,*,#2689,.T.);
#3322=ORIENTED_EDGE('',*,*,#2690,.F.);
#3323=ORIENTED_EDGE('',*,*,#2689,.F.);
#3324=ORIENTED_EDGE('',*,*,#2688,.T.);
#3325=ORIENTED_EDGE('',*,*,#2691,.F.);
#3326=ORIENTED_EDGE('',*,*,#2692,.T.);
#3327=ORIENTED_EDGE('',*,*,#2693,.F.);
#3328=ORIENTED_EDGE('',*,*,#2692,.F.);
#3329=ORIENTED_EDGE('',*,*,#2691,.T.);
#3330=ORIENTED_EDGE('',*,*,#2694,.F.);
#3331=ORIENTED_EDGE('',*,*,#2695,.T.);
#3332=ORIENTED_EDGE('',*,*,#2696,.F.);
#3333=ORIENTED_EDGE('',*,*,#2695,.F.);
#3334=ORIENTED_EDGE('',*,*,#2694,.T.);
#3335=ORIENTED_EDGE('',*,*,#2697,.F.);
#3336=ORIENTED_EDGE('',*,*,#2698,.T.);
#3337=ORIENTED_EDGE('',*,*,#2699,.T.);
#3338=ORIENTED_EDGE('',*,*,#2698,.F.);
#3339=ORIENTED_EDGE('',*,*,#2699,.F.);
#3340=ORIENTED_EDGE('',*,*,#2700,.F.);
#3341=ORIENTED_EDGE('',*,*,#2701,.T.);
#3342=ORIENTED_EDGE('',*,*,#2702,.T.);
#3343=ORIENTED_EDGE('',*,*,#2701,.F.);
#3344=ORIENTED_EDGE('',*,*,#2702,.F.);
#3345=ORIENTED_EDGE('',*,*,#2703,.F.);
#3346=ORIENTED_EDGE('',*,*,#2704,.T.);
#3347=ORIENTED_EDGE('',*,*,#2705,.T.);
#3348=ORIENTED_EDGE('',*,*,#2704,.F.);
#3349=ORIENTED_EDGE('',*,*,#2705,.F.);
#3350=ORIENTED_EDGE('',*,*,#2706,.F.);
#3351=ORIENTED_EDGE('',*,*,#2707,.T.);
#3352=ORIENTED_EDGE('',*,*,#2708,.T.);
#3353=ORIENTED_EDGE('',*,*,#2707,.F.);
#3354=ORIENTED_EDGE('',*,*,#2708,.F.);
#3355=ORIENTED_EDGE('',*,*,#2709,.F.);
#3356=ORIENTED_EDGE('',*,*,#2710,.F.);
#3357=ORIENTED_EDGE('',*,*,#2711,.T.);
#3358=ORIENTED_EDGE('',*,*,#2712,.F.);
#3359=ORIENTED_EDGE('',*,*,#2713,.F.);
#3360=ORIENTED_EDGE('',*,*,#2711,.F.);
#3361=ORIENTED_EDGE('',*,*,#2714,.F.);
#3362=ORIENTED_EDGE('',*,*,#2715,.T.);
#3363=ORIENTED_EDGE('',*,*,#2716,.F.);
#3364=ORIENTED_EDGE('',*,*,#2715,.F.);
#3365=ORIENTED_EDGE('',*,*,#2717,.F.);
#3366=ORIENTED_EDGE('',*,*,#2718,.T.);
#3367=ORIENTED_EDGE('',*,*,#2719,.F.);
#3368=ORIENTED_EDGE('',*,*,#2718,.F.);
#3369=ORIENTED_EDGE('',*,*,#2720,.F.);
#3370=ORIENTED_EDGE('',*,*,#2721,.T.);
#3371=ORIENTED_EDGE('',*,*,#2722,.F.);
#3372=ORIENTED_EDGE('',*,*,#2721,.F.);
#3373=ORIENTED_EDGE('',*,*,#2723,.F.);
#3374=ORIENTED_EDGE('',*,*,#2724,.T.);
#3375=ORIENTED_EDGE('',*,*,#2725,.F.);
#3376=ORIENTED_EDGE('',*,*,#2724,.F.);
#3377=ORIENTED_EDGE('',*,*,#2726,.F.);
#3378=ORIENTED_EDGE('',*,*,#2727,.T.);
#3379=ORIENTED_EDGE('',*,*,#2728,.T.);
#3380=ORIENTED_EDGE('',*,*,#2729,.T.);
#3381=ORIENTED_EDGE('',*,*,#2730,.F.);
#3382=ORIENTED_EDGE('',*,*,#2731,.T.);
#3383=ORIENTED_EDGE('',*,*,#2732,.T.);
#3384=ORIENTED_EDGE('',*,*,#2733,.T.);
#3385=ORIENTED_EDGE('',*,*,#2734,.F.);
#3386=ORIENTED_EDGE('',*,*,#2735,.T.);
#3387=ORIENTED_EDGE('',*,*,#2736,.T.);
#3388=ORIENTED_EDGE('',*,*,#2737,.T.);
#3389=ORIENTED_EDGE('',*,*,#2738,.F.);
#3390=ORIENTED_EDGE('',*,*,#2739,.T.);
#3391=ORIENTED_EDGE('',*,*,#2740,.T.);
#3392=ORIENTED_EDGE('',*,*,#2741,.T.);
#3393=ORIENTED_EDGE('',*,*,#2742,.F.);
#3394=ORIENTED_EDGE('',*,*,#2737,.F.);
#3395=ORIENTED_EDGE('',*,*,#2743,.T.);
#3396=ORIENTED_EDGE('',*,*,#2727,.F.);
#3397=ORIENTED_EDGE('',*,*,#2725,.T.);
#3398=ORIENTED_EDGE('',*,*,#2744,.F.);
#3399=ORIENTED_EDGE('',*,*,#2733,.F.);
#3400=ORIENTED_EDGE('',*,*,#2745,.F.);
#3401=ORIENTED_EDGE('',*,*,#2739,.F.);
#3402=ORIENTED_EDGE('',*,*,#2719,.T.);
#3403=ORIENTED_EDGE('',*,*,#2740,.F.);
#3404=ORIENTED_EDGE('',*,*,#2745,.T.);
#3405=ORIENTED_EDGE('',*,*,#2732,.F.);
#3406=ORIENTED_EDGE('',*,*,#2746,.F.);
#3407=ORIENTED_EDGE('',*,*,#2729,.F.);
#3408=ORIENTED_EDGE('',*,*,#2747,.F.);
#3409=ORIENTED_EDGE('',*,*,#2735,.F.);
#3410=ORIENTED_EDGE('',*,*,#2741,.F.);
#3411=ORIENTED_EDGE('',*,*,#2746,.T.);
#3412=ORIENTED_EDGE('',*,*,#2731,.F.);
#3413=ORIENTED_EDGE('',*,*,#2717,.T.);
#3414=ORIENTED_EDGE('',*,*,#2723,.T.);
#3415=ORIENTED_EDGE('',*,*,#2736,.F.);
#3416=ORIENTED_EDGE('',*,*,#2747,.T.);
#3417=ORIENTED_EDGE('',*,*,#2728,.F.);
#3418=ORIENTED_EDGE('',*,*,#2743,.F.);
#3419=ORIENTED_EDGE('',*,*,#2748,.F.);
#3420=ORIENTED_EDGE('',*,*,#2749,.T.);
#3421=ORIENTED_EDGE('',*,*,#2750,.T.);
#3422=ORIENTED_EDGE('',*,*,#2751,.T.);
#3423=ORIENTED_EDGE('',*,*,#2752,.F.);
#3424=ORIENTED_EDGE('',*,*,#2753,.T.);
#3425=ORIENTED_EDGE('',*,*,#2754,.T.);
#3426=ORIENTED_EDGE('',*,*,#2755,.T.);
#3427=ORIENTED_EDGE('',*,*,#2756,.F.);
#3428=ORIENTED_EDGE('',*,*,#2757,.T.);
#3429=ORIENTED_EDGE('',*,*,#2758,.T.);
#3430=ORIENTED_EDGE('',*,*,#2759,.T.);
#3431=ORIENTED_EDGE('',*,*,#2760,.F.);
#3432=ORIENTED_EDGE('',*,*,#2761,.T.);
#3433=ORIENTED_EDGE('',*,*,#2762,.T.);
#3434=ORIENTED_EDGE('',*,*,#2763,.T.);
#3435=ORIENTED_EDGE('',*,*,#2764,.F.);
#3436=ORIENTED_EDGE('',*,*,#2759,.F.);
#3437=ORIENTED_EDGE('',*,*,#2765,.T.);
#3438=ORIENTED_EDGE('',*,*,#2749,.F.);
#3439=ORIENTED_EDGE('',*,*,#2716,.T.);
#3440=ORIENTED_EDGE('',*,*,#2766,.F.);
#3441=ORIENTED_EDGE('',*,*,#2755,.F.);
#3442=ORIENTED_EDGE('',*,*,#2767,.F.);
#3443=ORIENTED_EDGE('',*,*,#2761,.F.);
#3444=ORIENTED_EDGE('',*,*,#2722,.T.);
#3445=ORIENTED_EDGE('',*,*,#2762,.F.);
#3446=ORIENTED_EDGE('',*,*,#2767,.T.);
#3447=ORIENTED_EDGE('',*,*,#2754,.F.);
#3448=ORIENTED_EDGE('',*,*,#2768,.F.);
#3449=ORIENTED_EDGE('',*,*,#2751,.F.);
#3450=ORIENTED_EDGE('',*,*,#2769,.F.);
#3451=ORIENTED_EDGE('',*,*,#2757,.F.);
#3452=ORIENTED_EDGE('',*,*,#2763,.F.);
#3453=ORIENTED_EDGE('',*,*,#2768,.T.);
#3454=ORIENTED_EDGE('',*,*,#2753,.F.);
#3455=ORIENTED_EDGE('',*,*,#2714,.T.);
#3456=ORIENTED_EDGE('',*,*,#2720,.T.);
#3457=ORIENTED_EDGE('',*,*,#2758,.F.);
#3458=ORIENTED_EDGE('',*,*,#2769,.T.);
#3459=ORIENTED_EDGE('',*,*,#2750,.F.);
#3460=ORIENTED_EDGE('',*,*,#2765,.F.);
#3461=ORIENTED_EDGE('',*,*,#2770,.F.);
#3462=ORIENTED_EDGE('',*,*,#2771,.T.);
#3463=ORIENTED_EDGE('',*,*,#2772,.T.);
#3464=ORIENTED_EDGE('',*,*,#2771,.F.);
#3465=ORIENTED_EDGE('',*,*,#2709,.T.);
#3466=ORIENTED_EDGE('',*,*,#2710,.T.);
#3467=ORIENTED_EDGE('',*,*,#2773,.F.);
#3468=ORIENTED_EDGE('',*,*,#2774,.T.);
#3469=ORIENTED_EDGE('',*,*,#2775,.T.);
#3470=ORIENTED_EDGE('',*,*,#2774,.F.);
#3471=ORIENTED_EDGE('',*,*,#2712,.T.);
#3472=ORIENTED_EDGE('',*,*,#2713,.T.);
#3473=ORIENTED_EDGE('',*,*,#2742,.T.);
#3474=ORIENTED_EDGE('',*,*,#2726,.T.);
#3475=ORIENTED_EDGE('',*,*,#2730,.T.);
#3476=ORIENTED_EDGE('',*,*,#2744,.T.);
#3477=ORIENTED_EDGE('',*,*,#2738,.T.);
#3478=ORIENTED_EDGE('',*,*,#2734,.T.);
#3479=ORIENTED_EDGE('',*,*,#2764,.T.);
#3480=ORIENTED_EDGE('',*,*,#2748,.T.);
#3481=ORIENTED_EDGE('',*,*,#2752,.T.);
#3482=ORIENTED_EDGE('',*,*,#2766,.T.);
#3483=ORIENTED_EDGE('',*,*,#2760,.T.);
#3484=ORIENTED_EDGE('',*,*,#2756,.T.);
#3485=ORIENTED_EDGE('',*,*,#2773,.T.);
#3486=ORIENTED_EDGE('',*,*,#2770,.T.);
#3487=ORIENTED_EDGE('',*,*,#2696,.T.);
#3488=ORIENTED_EDGE('',*,*,#2693,.T.);
#3489=ORIENTED_EDGE('',*,*,#2690,.T.);
#3490=ORIENTED_EDGE('',*,*,#2687,.T.);
#3491=ORIENTED_EDGE('',*,*,#2775,.F.);
#3492=ORIENTED_EDGE('',*,*,#2772,.F.);
#3493=ORIENTED_EDGE('',*,*,#2706,.T.);
#3494=ORIENTED_EDGE('',*,*,#2703,.T.);
#3495=ORIENTED_EDGE('',*,*,#2700,.T.);
#3496=ORIENTED_EDGE('',*,*,#2697,.T.);
#3497=ORIENTED_EDGE('',*,*,#2776,.F.);
#3498=ORIENTED_EDGE('',*,*,#2777,.T.);
#3499=ORIENTED_EDGE('',*,*,#2778,.T.);
#3500=ORIENTED_EDGE('',*,*,#2777,.F.);
#3501=ORIENTED_EDGE('',*,*,#2778,.F.);
#3502=ORIENTED_EDGE('',*,*,#2779,.F.);
#3503=ORIENTED_EDGE('',*,*,#2776,.T.);
#3504=ORIENTED_EDGE('',*,*,#2780,.F.);
#3505=ORIENTED_EDGE('',*,*,#2780,.T.);
#3506=ORIENTED_EDGE('',*,*,#2781,.T.);
#3507=ORIENTED_EDGE('',*,*,#2782,.T.);
#3508=ORIENTED_EDGE('',*,*,#2781,.F.);
#3509=ORIENTED_EDGE('',*,*,#2783,.F.);
#3510=ORIENTED_EDGE('',*,*,#2784,.T.);
#3511=ORIENTED_EDGE('',*,*,#2779,.T.);
#3512=ORIENTED_EDGE('',*,*,#2784,.F.);
#3513=ORIENTED_EDGE('',*,*,#2785,.F.);
#3514=ORIENTED_EDGE('',*,*,#2786,.T.);
#3515=ORIENTED_EDGE('',*,*,#2787,.T.);
#3516=ORIENTED_EDGE('',*,*,#2786,.F.);
#3517=ORIENTED_EDGE('',*,*,#2785,.T.);
#3518=ORIENTED_EDGE('',*,*,#2783,.T.);
#3519=ORIENTED_EDGE('',*,*,#2787,.F.);
#3520=ORIENTED_EDGE('',*,*,#2782,.F.);
#3521=ORIENTED_EDGE('',*,*,#2788,.F.);
#3522=ORIENTED_EDGE('',*,*,#2789,.T.);
#3523=ORIENTED_EDGE('',*,*,#2788,.T.);
#3524=ORIENTED_EDGE('',*,*,#2789,.F.);
#3525=ORIENTED_EDGE('',*,*,#2790,.F.);
#3526=ORIENTED_EDGE('',*,*,#2791,.T.);
#3527=ORIENTED_EDGE('',*,*,#2792,.T.);
#3528=ORIENTED_EDGE('',*,*,#2791,.F.);
#3529=ORIENTED_EDGE('',*,*,#2792,.F.);
#3530=ORIENTED_EDGE('',*,*,#2793,.F.);
#3531=ORIENTED_EDGE('',*,*,#2790,.T.);
#3532=ORIENTED_EDGE('',*,*,#2794,.F.);
#3533=ORIENTED_EDGE('',*,*,#2794,.T.);
#3534=ORIENTED_EDGE('',*,*,#2795,.T.);
#3535=ORIENTED_EDGE('',*,*,#2796,.T.);
#3536=ORIENTED_EDGE('',*,*,#2795,.F.);
#3537=ORIENTED_EDGE('',*,*,#2797,.F.);
#3538=ORIENTED_EDGE('',*,*,#2798,.T.);
#3539=ORIENTED_EDGE('',*,*,#2793,.T.);
#3540=ORIENTED_EDGE('',*,*,#2798,.F.);
#3541=ORIENTED_EDGE('',*,*,#2799,.F.);
#3542=ORIENTED_EDGE('',*,*,#2800,.T.);
#3543=ORIENTED_EDGE('',*,*,#2801,.T.);
#3544=ORIENTED_EDGE('',*,*,#2800,.F.);
#3545=ORIENTED_EDGE('',*,*,#2799,.T.);
#3546=ORIENTED_EDGE('',*,*,#2797,.T.);
#3547=ORIENTED_EDGE('',*,*,#2801,.F.);
#3548=ORIENTED_EDGE('',*,*,#2796,.F.);
#3549=ORIENTED_EDGE('',*,*,#2802,.F.);
#3550=ORIENTED_EDGE('',*,*,#2803,.T.);
#3551=ORIENTED_EDGE('',*,*,#2802,.T.);
#3552=ORIENTED_EDGE('',*,*,#2803,.F.);
#3553=ORIENTED_EDGE('',*,*,#2804,.F.);
#3554=ORIENTED_EDGE('',*,*,#2805,.F.);
#3555=ORIENTED_EDGE('',*,*,#2806,.F.);
#3556=ORIENTED_EDGE('',*,*,#2807,.F.);
#3557=ORIENTED_EDGE('',*,*,#2808,.F.);
#3558=ORIENTED_EDGE('',*,*,#2809,.F.);
#3559=ORIENTED_EDGE('',*,*,#2810,.F.);
#3560=ORIENTED_EDGE('',*,*,#2811,.F.);
#3561=ORIENTED_EDGE('',*,*,#2812,.F.);
#3562=ORIENTED_EDGE('',*,*,#2807,.T.);
#3563=ORIENTED_EDGE('',*,*,#2813,.F.);
#3564=ORIENTED_EDGE('',*,*,#2809,.T.);
#3565=ORIENTED_EDGE('',*,*,#2814,.F.);
#3566=ORIENTED_EDGE('',*,*,#2810,.T.);
#3567=ORIENTED_EDGE('',*,*,#2813,.T.);
#3568=ORIENTED_EDGE('',*,*,#2806,.T.);
#3569=ORIENTED_EDGE('',*,*,#2815,.T.);
#3570=ORIENTED_EDGE('',*,*,#2816,.T.);
#3571=ORIENTED_EDGE('',*,*,#2811,.T.);
#3572=ORIENTED_EDGE('',*,*,#2815,.F.);
#3573=ORIENTED_EDGE('',*,*,#2805,.T.);
#3574=ORIENTED_EDGE('',*,*,#2817,.T.);
#3575=ORIENTED_EDGE('',*,*,#2818,.F.);
#3576=ORIENTED_EDGE('',*,*,#2819,.F.);
#3577=ORIENTED_EDGE('',*,*,#2820,.T.);
#3578=ORIENTED_EDGE('',*,*,#2814,.T.);
#3579=ORIENTED_EDGE('',*,*,#2820,.F.);
#3580=ORIENTED_EDGE('',*,*,#2816,.F.);
#3581=ORIENTED_EDGE('',*,*,#2821,.T.);
#3582=ORIENTED_EDGE('',*,*,#2822,.T.);
#3583=ORIENTED_EDGE('',*,*,#2821,.F.);
#3584=ORIENTED_EDGE('',*,*,#2818,.T.);
#3585=ORIENTED_EDGE('',*,*,#2819,.T.);
#3586=ORIENTED_EDGE('',*,*,#2808,.T.);
#3587=ORIENTED_EDGE('',*,*,#2817,.F.);
#3588=ORIENTED_EDGE('',*,*,#2804,.T.);
#3589=ORIENTED_EDGE('',*,*,#2812,.T.);
#3590=ORIENTED_EDGE('',*,*,#2822,.F.);
#3591=ORIENTED_EDGE('',*,*,#2823,.F.);
#3592=ORIENTED_EDGE('',*,*,#2824,.T.);
#3593=ORIENTED_EDGE('',*,*,#2825,.F.);
#3594=ORIENTED_EDGE('',*,*,#2824,.F.);
#3595=ORIENTED_EDGE('',*,*,#2826,.F.);
#3596=ORIENTED_EDGE('',*,*,#2827,.T.);
#3597=ORIENTED_EDGE('',*,*,#2828,.F.);
#3598=ORIENTED_EDGE('',*,*,#2827,.F.);
#3599=ORIENTED_EDGE('',*,*,#2829,.F.);
#3600=ORIENTED_EDGE('',*,*,#2830,.T.);
#3601=ORIENTED_EDGE('',*,*,#2831,.F.);
#3602=ORIENTED_EDGE('',*,*,#2830,.F.);
#3603=ORIENTED_EDGE('',*,*,#2832,.F.);
#3604=ORIENTED_EDGE('',*,*,#2833,.T.);
#3605=ORIENTED_EDGE('',*,*,#2834,.F.);
#3606=ORIENTED_EDGE('',*,*,#2833,.F.);
#3607=ORIENTED_EDGE('',*,*,#2835,.F.);
#3608=ORIENTED_EDGE('',*,*,#2836,.T.);
#3609=ORIENTED_EDGE('',*,*,#2837,.F.);
#3610=ORIENTED_EDGE('',*,*,#2836,.F.);
#3611=ORIENTED_EDGE('',*,*,#2835,.T.);
#3612=ORIENTED_EDGE('',*,*,#2838,.T.);
#3613=ORIENTED_EDGE('',*,*,#2838,.F.);
#3614=ORIENTED_EDGE('',*,*,#2839,.T.);
#3615=ORIENTED_EDGE('',*,*,#2840,.T.);
#3616=ORIENTED_EDGE('',*,*,#2839,.F.);
#3617=ORIENTED_EDGE('',*,*,#2841,.F.);
#3618=ORIENTED_EDGE('',*,*,#2842,.T.);
#3619=ORIENTED_EDGE('',*,*,#2843,.T.);
#3620=ORIENTED_EDGE('',*,*,#2842,.F.);
#3621=ORIENTED_EDGE('',*,*,#2841,.T.);
#3622=ORIENTED_EDGE('',*,*,#2837,.T.);
#3623=ORIENTED_EDGE('',*,*,#2834,.T.);
#3624=ORIENTED_EDGE('',*,*,#2831,.T.);
#3625=ORIENTED_EDGE('',*,*,#2828,.T.);
#3626=ORIENTED_EDGE('',*,*,#2825,.T.);
#3627=ORIENTED_EDGE('',*,*,#2843,.F.);
#3628=ORIENTED_EDGE('',*,*,#2840,.F.);
#3629=ORIENTED_EDGE('',*,*,#2832,.T.);
#3630=ORIENTED_EDGE('',*,*,#2829,.T.);
#3631=ORIENTED_EDGE('',*,*,#2826,.T.);
#3632=ORIENTED_EDGE('',*,*,#2823,.T.);
#3633=ORIENTED_EDGE('',*,*,#2844,.F.);
#3634=ORIENTED_EDGE('',*,*,#2845,.T.);
#3635=ORIENTED_EDGE('',*,*,#2846,.F.);
#3636=ORIENTED_EDGE('',*,*,#2845,.F.);
#3637=ORIENTED_EDGE('',*,*,#2847,.F.);
#3638=ORIENTED_EDGE('',*,*,#2848,.T.);
#3639=ORIENTED_EDGE('',*,*,#2849,.F.);
#3640=ORIENTED_EDGE('',*,*,#2848,.F.);
#3641=ORIENTED_EDGE('',*,*,#2850,.F.);
#3642=ORIENTED_EDGE('',*,*,#2851,.T.);
#3643=ORIENTED_EDGE('',*,*,#2852,.F.);
#3644=ORIENTED_EDGE('',*,*,#2851,.F.);
#3645=ORIENTED_EDGE('',*,*,#2853,.F.);
#3646=ORIENTED_EDGE('',*,*,#2854,.T.);
#3647=ORIENTED_EDGE('',*,*,#2855,.F.);
#3648=ORIENTED_EDGE('',*,*,#2854,.F.);
#3649=ORIENTED_EDGE('',*,*,#2856,.F.);
#3650=ORIENTED_EDGE('',*,*,#2857,.T.);
#3651=ORIENTED_EDGE('',*,*,#2858,.T.);
#3652=ORIENTED_EDGE('',*,*,#2857,.F.);
#3653=ORIENTED_EDGE('',*,*,#2858,.F.);
#3654=ORIENTED_EDGE('',*,*,#2859,.F.);
#3655=ORIENTED_EDGE('',*,*,#2860,.F.);
#3656=ORIENTED_EDGE('',*,*,#2861,.T.);
#3657=ORIENTED_EDGE('',*,*,#2859,.T.);
#3658=ORIENTED_EDGE('',*,*,#2861,.F.);
#3659=ORIENTED_EDGE('',*,*,#2862,.F.);
#3660=ORIENTED_EDGE('',*,*,#2863,.T.);
#3661=ORIENTED_EDGE('',*,*,#2864,.T.);
#3662=ORIENTED_EDGE('',*,*,#2863,.F.);
#3663=ORIENTED_EDGE('',*,*,#2862,.T.);
#3664=ORIENTED_EDGE('',*,*,#2860,.T.);
#3665=ORIENTED_EDGE('',*,*,#2855,.T.);
#3666=ORIENTED_EDGE('',*,*,#2852,.T.);
#3667=ORIENTED_EDGE('',*,*,#2849,.T.);
#3668=ORIENTED_EDGE('',*,*,#2846,.T.);
#3669=ORIENTED_EDGE('',*,*,#2864,.F.);
#3670=ORIENTED_EDGE('',*,*,#2856,.T.);
#3671=ORIENTED_EDGE('',*,*,#2853,.T.);
#3672=ORIENTED_EDGE('',*,*,#2850,.T.);
#3673=ORIENTED_EDGE('',*,*,#2847,.T.);
#3674=ORIENTED_EDGE('',*,*,#2844,.T.);
#3675=ORIENTED_EDGE('',*,*,#2865,.T.);
#3676=ORIENTED_EDGE('',*,*,#2866,.T.);
#3677=ORIENTED_EDGE('',*,*,#2867,.F.);
#3678=ORIENTED_EDGE('',*,*,#2868,.F.);
#3679=ORIENTED_EDGE('',*,*,#2869,.T.);
#3680=ORIENTED_EDGE('',*,*,#2868,.T.);
#3681=ORIENTED_EDGE('',*,*,#2870,.F.);
#3682=ORIENTED_EDGE('',*,*,#2871,.F.);
#3683=ORIENTED_EDGE('',*,*,#2872,.T.);
#3684=ORIENTED_EDGE('',*,*,#2871,.T.);
#3685=ORIENTED_EDGE('',*,*,#2873,.F.);
#3686=ORIENTED_EDGE('',*,*,#2874,.F.);
#3687=ORIENTED_EDGE('',*,*,#2875,.T.);
#3688=ORIENTED_EDGE('',*,*,#2874,.T.);
#3689=ORIENTED_EDGE('',*,*,#2876,.F.);
#3690=ORIENTED_EDGE('',*,*,#2866,.F.);
#3691=ORIENTED_EDGE('',*,*,#2876,.T.);
#3692=ORIENTED_EDGE('',*,*,#2873,.T.);
#3693=ORIENTED_EDGE('',*,*,#2870,.T.);
#3694=ORIENTED_EDGE('',*,*,#2867,.T.);
#3695=ORIENTED_EDGE('',*,*,#2875,.F.);
#3696=ORIENTED_EDGE('',*,*,#2865,.F.);
#3697=ORIENTED_EDGE('',*,*,#2869,.F.);
#3698=ORIENTED_EDGE('',*,*,#2872,.F.);
#3699=ORIENTED_EDGE('',*,*,#2877,.T.);
#3700=ORIENTED_EDGE('',*,*,#2878,.T.);
#3701=ORIENTED_EDGE('',*,*,#2879,.F.);
#3702=ORIENTED_EDGE('',*,*,#2880,.F.);
#3703=ORIENTED_EDGE('',*,*,#2881,.T.);
#3704=ORIENTED_EDGE('',*,*,#2880,.T.);
#3705=ORIENTED_EDGE('',*,*,#2882,.F.);
#3706=ORIENTED_EDGE('',*,*,#2883,.F.);
#3707=ORIENTED_EDGE('',*,*,#2884,.T.);
#3708=ORIENTED_EDGE('',*,*,#2883,.T.);
#3709=ORIENTED_EDGE('',*,*,#2885,.F.);
#3710=ORIENTED_EDGE('',*,*,#2886,.F.);
#3711=ORIENTED_EDGE('',*,*,#2887,.T.);
#3712=ORIENTED_EDGE('',*,*,#2886,.T.);
#3713=ORIENTED_EDGE('',*,*,#2888,.F.);
#3714=ORIENTED_EDGE('',*,*,#2878,.F.);
#3715=ORIENTED_EDGE('',*,*,#2888,.T.);
#3716=ORIENTED_EDGE('',*,*,#2885,.T.);
#3717=ORIENTED_EDGE('',*,*,#2882,.T.);
#3718=ORIENTED_EDGE('',*,*,#2879,.T.);
#3719=ORIENTED_EDGE('',*,*,#2887,.F.);
#3720=ORIENTED_EDGE('',*,*,#2877,.F.);
#3721=ORIENTED_EDGE('',*,*,#2881,.F.);
#3722=ORIENTED_EDGE('',*,*,#2884,.F.);
#3723=ORIENTED_EDGE('',*,*,#2889,.F.);
#3724=ORIENTED_EDGE('',*,*,#2890,.F.);
#3725=ORIENTED_EDGE('',*,*,#2891,.T.);
#3726=ORIENTED_EDGE('',*,*,#2892,.F.);
#3727=ORIENTED_EDGE('',*,*,#2893,.F.);
#3728=ORIENTED_EDGE('',*,*,#2891,.F.);
#3729=ORIENTED_EDGE('',*,*,#2892,.T.);
#3730=ORIENTED_EDGE('',*,*,#2893,.T.);
#3731=ORIENTED_EDGE('',*,*,#2894,.T.);
#3732=ORIENTED_EDGE('',*,*,#2895,.T.);
#3733=ORIENTED_EDGE('',*,*,#2894,.F.);
#3734=ORIENTED_EDGE('',*,*,#2896,.T.);
#3735=ORIENTED_EDGE('',*,*,#2897,.T.);
#3736=ORIENTED_EDGE('',*,*,#2898,.F.);
#3737=ORIENTED_EDGE('',*,*,#2897,.F.);
#3738=ORIENTED_EDGE('',*,*,#2898,.T.);
#3739=ORIENTED_EDGE('',*,*,#2899,.T.);
#3740=ORIENTED_EDGE('',*,*,#2900,.F.);
#3741=ORIENTED_EDGE('',*,*,#2899,.F.);
#3742=ORIENTED_EDGE('',*,*,#2895,.F.);
#3743=ORIENTED_EDGE('',*,*,#2900,.T.);
#3744=ORIENTED_EDGE('',*,*,#2901,.F.);
#3745=ORIENTED_EDGE('',*,*,#2902,.T.);
#3746=ORIENTED_EDGE('',*,*,#2889,.T.);
#3747=ORIENTED_EDGE('',*,*,#2890,.T.);
#3748=ORIENTED_EDGE('',*,*,#2902,.F.);
#3749=ORIENTED_EDGE('',*,*,#2901,.T.);
#3750=ORIENTED_EDGE('',*,*,#2903,.F.);
#3751=ORIENTED_EDGE('',*,*,#2903,.T.);
#3752=ORIENTED_EDGE('',*,*,#2904,.T.);
#3753=ORIENTED_EDGE('',*,*,#2896,.F.);
#3754=ORIENTED_EDGE('',*,*,#2904,.F.);
#3755=ORIENTED_EDGE('',*,*,#2905,.F.);
#3756=ORIENTED_EDGE('',*,*,#2906,.F.);
#3757=ORIENTED_EDGE('',*,*,#2907,.T.);
#3758=ORIENTED_EDGE('',*,*,#2908,.F.);
#3759=ORIENTED_EDGE('',*,*,#2909,.F.);
#3760=ORIENTED_EDGE('',*,*,#2907,.F.);
#3761=ORIENTED_EDGE('',*,*,#2910,.T.);
#3762=ORIENTED_EDGE('',*,*,#2911,.T.);
#3763=ORIENTED_EDGE('',*,*,#2908,.T.);
#3764=ORIENTED_EDGE('',*,*,#2909,.T.);
#3765=ORIENTED_EDGE('',*,*,#2911,.F.);
#3766=ORIENTED_EDGE('',*,*,#2912,.F.);
#3767=ORIENTED_EDGE('',*,*,#2913,.T.);
#3768=ORIENTED_EDGE('',*,*,#2914,.F.);
#3769=ORIENTED_EDGE('',*,*,#2915,.T.);
#3770=ORIENTED_EDGE('',*,*,#2912,.T.);
#3771=ORIENTED_EDGE('',*,*,#2915,.F.);
#3772=ORIENTED_EDGE('',*,*,#2916,.F.);
#3773=ORIENTED_EDGE('',*,*,#2917,.T.);
#3774=ORIENTED_EDGE('',*,*,#2914,.T.);
#3775=ORIENTED_EDGE('',*,*,#2917,.F.);
#3776=ORIENTED_EDGE('',*,*,#2918,.F.);
#3777=ORIENTED_EDGE('',*,*,#2919,.T.);
#3778=ORIENTED_EDGE('',*,*,#2916,.T.);
#3779=ORIENTED_EDGE('',*,*,#2919,.F.);
#3780=ORIENTED_EDGE('',*,*,#2918,.T.);
#3781=ORIENTED_EDGE('',*,*,#2910,.F.);
#3782=ORIENTED_EDGE('',*,*,#2905,.T.);
#3783=ORIENTED_EDGE('',*,*,#2906,.T.);
#3784=ORIENTED_EDGE('',*,*,#2920,.T.);
#3785=ORIENTED_EDGE('',*,*,#2913,.F.);
#3786=ORIENTED_EDGE('',*,*,#2920,.F.);
#3787=ORIENTED_EDGE('',*,*,#2921,.T.);
#3788=ORIENTED_EDGE('',*,*,#2921,.F.);
#3789=ORIENTED_EDGE('',*,*,#2922,.T.);
#3790=ORIENTED_EDGE('',*,*,#2922,.F.);
#3791=ORIENTED_EDGE('',*,*,#2923,.T.);
#3792=ORIENTED_EDGE('',*,*,#2923,.F.);
#3793=ORIENTED_EDGE('',*,*,#2924,.T.);
#3794=ORIENTED_EDGE('',*,*,#2924,.F.);
#3795=ORIENTED_EDGE('',*,*,#2925,.T.);
#3796=ORIENTED_EDGE('',*,*,#2925,.F.);
#3797=ORIENTED_EDGE('',*,*,#2926,.T.);
#3798=ORIENTED_EDGE('',*,*,#2926,.F.);
#3799=ORIENTED_EDGE('',*,*,#2927,.T.);
#3800=ORIENTED_EDGE('',*,*,#2927,.F.);
#3801=ORIENTED_EDGE('',*,*,#2928,.T.);
#3802=ORIENTED_EDGE('',*,*,#2928,.F.);
#3803=ORIENTED_EDGE('',*,*,#2929,.F.);
#3804=ORIENTED_EDGE('',*,*,#2930,.F.);
#3805=ORIENTED_EDGE('',*,*,#2931,.F.);
#3806=ORIENTED_EDGE('',*,*,#2932,.F.);
#3807=ORIENTED_EDGE('',*,*,#2931,.T.);
#3808=ORIENTED_EDGE('',*,*,#2933,.F.);
#3809=ORIENTED_EDGE('',*,*,#2934,.T.);
#3810=ORIENTED_EDGE('',*,*,#2935,.F.);
#3811=ORIENTED_EDGE('',*,*,#2936,.T.);
#3812=ORIENTED_EDGE('',*,*,#2937,.F.);
#3813=ORIENTED_EDGE('',*,*,#2938,.T.);
#3814=ORIENTED_EDGE('',*,*,#2939,.T.);
#3815=ORIENTED_EDGE('',*,*,#2940,.F.);
#3816=ORIENTED_EDGE('',*,*,#2939,.F.);
#3817=ORIENTED_EDGE('',*,*,#2941,.T.);
#3818=ORIENTED_EDGE('',*,*,#2942,.F.);
#3819=ORIENTED_EDGE('',*,*,#2943,.T.);
#3820=ORIENTED_EDGE('',*,*,#2944,.F.);
#3821=ORIENTED_EDGE('',*,*,#2945,.T.);
#3822=ORIENTED_EDGE('',*,*,#2946,.F.);
#3823=ORIENTED_EDGE('',*,*,#2947,.T.);
#3824=ORIENTED_EDGE('',*,*,#2948,.F.);
#3825=ORIENTED_EDGE('',*,*,#2949,.T.);
#3826=ORIENTED_EDGE('',*,*,#2950,.F.);
#3827=ORIENTED_EDGE('',*,*,#2930,.T.);
#3828=ORIENTED_EDGE('',*,*,#2951,.T.);
#3829=ORIENTED_EDGE('',*,*,#2952,.T.);
#3830=ORIENTED_EDGE('',*,*,#2933,.T.);
#3831=ORIENTED_EDGE('',*,*,#2953,.F.);
#3832=ORIENTED_EDGE('',*,*,#2954,.F.);
#3833=ORIENTED_EDGE('',*,*,#2934,.F.);
#3834=ORIENTED_EDGE('',*,*,#2952,.F.);
#3835=ORIENTED_EDGE('',*,*,#2954,.T.);
#3836=ORIENTED_EDGE('',*,*,#2955,.T.);
#3837=ORIENTED_EDGE('',*,*,#2956,.T.);
#3838=ORIENTED_EDGE('',*,*,#2935,.T.);
#3839=ORIENTED_EDGE('',*,*,#2957,.F.);
#3840=ORIENTED_EDGE('',*,*,#2958,.F.);
#3841=ORIENTED_EDGE('',*,*,#2936,.F.);
#3842=ORIENTED_EDGE('',*,*,#2956,.F.);
#3843=ORIENTED_EDGE('',*,*,#2958,.T.);
#3844=ORIENTED_EDGE('',*,*,#2959,.T.);
#3845=ORIENTED_EDGE('',*,*,#2960,.T.);
#3846=ORIENTED_EDGE('',*,*,#2937,.T.);
#3847=ORIENTED_EDGE('',*,*,#2961,.F.);
#3848=ORIENTED_EDGE('',*,*,#2962,.F.);
#3849=ORIENTED_EDGE('',*,*,#2941,.F.);
#3850=ORIENTED_EDGE('',*,*,#2938,.F.);
#3851=ORIENTED_EDGE('',*,*,#2960,.F.);
#3852=ORIENTED_EDGE('',*,*,#2963,.F.);
#3853=ORIENTED_EDGE('',*,*,#2962,.T.);
#3854=ORIENTED_EDGE('',*,*,#2964,.T.);
#3855=ORIENTED_EDGE('',*,*,#2965,.T.);
#3856=ORIENTED_EDGE('',*,*,#2942,.T.);
#3857=ORIENTED_EDGE('',*,*,#2966,.F.);
#3858=ORIENTED_EDGE('',*,*,#2967,.F.);
#3859=ORIENTED_EDGE('',*,*,#2943,.F.);
#3860=ORIENTED_EDGE('',*,*,#2965,.F.);
#3861=ORIENTED_EDGE('',*,*,#2967,.T.);
#3862=ORIENTED_EDGE('',*,*,#2968,.T.);
#3863=ORIENTED_EDGE('',*,*,#2969,.T.);
#3864=ORIENTED_EDGE('',*,*,#2944,.T.);
#3865=ORIENTED_EDGE('',*,*,#2970,.F.);
#3866=ORIENTED_EDGE('',*,*,#2971,.F.);
#3867=ORIENTED_EDGE('',*,*,#2945,.F.);
#3868=ORIENTED_EDGE('',*,*,#2969,.F.);
#3869=ORIENTED_EDGE('',*,*,#2971,.T.);
#3870=ORIENTED_EDGE('',*,*,#2972,.T.);
#3871=ORIENTED_EDGE('',*,*,#2973,.T.);
#3872=ORIENTED_EDGE('',*,*,#2946,.T.);
#3873=ORIENTED_EDGE('',*,*,#2947,.F.);
#3874=ORIENTED_EDGE('',*,*,#2973,.F.);
#3875=ORIENTED_EDGE('',*,*,#2974,.F.);
#3876=ORIENTED_EDGE('',*,*,#2975,.F.);
#3877=ORIENTED_EDGE('',*,*,#2976,.F.);
#3878=ORIENTED_EDGE('',*,*,#2977,.T.);
#3879=ORIENTED_EDGE('',*,*,#2963,.T.);
#3880=ORIENTED_EDGE('',*,*,#2959,.F.);
#3881=ORIENTED_EDGE('',*,*,#2957,.T.);
#3882=ORIENTED_EDGE('',*,*,#2955,.F.);
#3883=ORIENTED_EDGE('',*,*,#2953,.T.);
#3884=ORIENTED_EDGE('',*,*,#2951,.F.);
#3885=ORIENTED_EDGE('',*,*,#2929,.T.);
#3886=ORIENTED_EDGE('',*,*,#2978,.F.);
#3887=ORIENTED_EDGE('',*,*,#2979,.T.);
#3888=ORIENTED_EDGE('',*,*,#2980,.F.);
#3889=ORIENTED_EDGE('',*,*,#2974,.T.);
#3890=ORIENTED_EDGE('',*,*,#2972,.F.);
#3891=ORIENTED_EDGE('',*,*,#2970,.T.);
#3892=ORIENTED_EDGE('',*,*,#2968,.F.);
#3893=ORIENTED_EDGE('',*,*,#2966,.T.);
#3894=ORIENTED_EDGE('',*,*,#2964,.F.);
#3895=ORIENTED_EDGE('',*,*,#2961,.T.);
#3896=ORIENTED_EDGE('',*,*,#2977,.F.);
#3897=ORIENTED_EDGE('',*,*,#2932,.T.);
#3898=ORIENTED_EDGE('',*,*,#2950,.T.);
#3899=ORIENTED_EDGE('',*,*,#2981,.T.);
#3900=ORIENTED_EDGE('',*,*,#2978,.T.);
#3901=ORIENTED_EDGE('',*,*,#2949,.F.);
#3902=ORIENTED_EDGE('',*,*,#2982,.F.);
#3903=ORIENTED_EDGE('',*,*,#2979,.F.);
#3904=ORIENTED_EDGE('',*,*,#2981,.F.);
#3905=ORIENTED_EDGE('',*,*,#2940,.T.);
#3906=ORIENTED_EDGE('',*,*,#2976,.T.);
#3907=ORIENTED_EDGE('',*,*,#2975,.T.);
#3908=ORIENTED_EDGE('',*,*,#2980,.T.);
#3909=ORIENTED_EDGE('',*,*,#2982,.T.);
#3910=ORIENTED_EDGE('',*,*,#2948,.T.);
#3911=ORIENTED_EDGE('',*,*,#2983,.F.);
#3912=ORIENTED_EDGE('',*,*,#2984,.T.);
#3913=ORIENTED_EDGE('',*,*,#2985,.F.);
#3914=ORIENTED_EDGE('',*,*,#2986,.T.);
#3915=ORIENTED_EDGE('',*,*,#2983,.T.);
#3916=ORIENTED_EDGE('',*,*,#2986,.F.);
#3917=ORIENTED_EDGE('',*,*,#2985,.T.);
#3918=ORIENTED_EDGE('',*,*,#2987,.F.);
#3919=ORIENTED_EDGE('',*,*,#2987,.T.);
#3920=ORIENTED_EDGE('',*,*,#2988,.T.);
#3921=ORIENTED_EDGE('',*,*,#2984,.F.);
#3922=ORIENTED_EDGE('',*,*,#2988,.F.);
#3923=ORIENTED_EDGE('',*,*,#2989,.F.);
#3924=ORIENTED_EDGE('',*,*,#2990,.T.);
#3925=ORIENTED_EDGE('',*,*,#2991,.F.);
#3926=ORIENTED_EDGE('',*,*,#2992,.T.);
#3927=ORIENTED_EDGE('',*,*,#2989,.T.);
#3928=ORIENTED_EDGE('',*,*,#2992,.F.);
#3929=ORIENTED_EDGE('',*,*,#2991,.T.);
#3930=ORIENTED_EDGE('',*,*,#2993,.F.);
#3931=ORIENTED_EDGE('',*,*,#2993,.T.);
#3932=ORIENTED_EDGE('',*,*,#2994,.T.);
#3933=ORIENTED_EDGE('',*,*,#2990,.F.);
#3934=ORIENTED_EDGE('',*,*,#2994,.F.);
#3935=ORIENTED_EDGE('',*,*,#2995,.F.);
#3936=ORIENTED_EDGE('',*,*,#2996,.F.);
#3937=ORIENTED_EDGE('',*,*,#2997,.T.);
#3938=ORIENTED_EDGE('',*,*,#2995,.T.);
#3939=ORIENTED_EDGE('',*,*,#2997,.F.);
#3940=ORIENTED_EDGE('',*,*,#2998,.F.);
#3941=ORIENTED_EDGE('',*,*,#2999,.T.);
#3942=ORIENTED_EDGE('',*,*,#2996,.T.);
#3943=ORIENTED_EDGE('',*,*,#2999,.F.);
#3944=ORIENTED_EDGE('',*,*,#3000,.F.);
#3945=ORIENTED_EDGE('',*,*,#3001,.T.);
#3946=ORIENTED_EDGE('',*,*,#2998,.T.);
#3947=ORIENTED_EDGE('',*,*,#3001,.F.);
#3948=ORIENTED_EDGE('',*,*,#3000,.T.);
#3949=ORIENTED_EDGE('',*,*,#3002,.F.);
#3950=ORIENTED_EDGE('',*,*,#3003,.F.);
#3951=ORIENTED_EDGE('',*,*,#3004,.T.);
#3952=ORIENTED_EDGE('',*,*,#3002,.T.);
#3953=ORIENTED_EDGE('',*,*,#3004,.F.);
#3954=ORIENTED_EDGE('',*,*,#3005,.F.);
#3955=ORIENTED_EDGE('',*,*,#3006,.T.);
#3956=ORIENTED_EDGE('',*,*,#3003,.T.);
#3957=ORIENTED_EDGE('',*,*,#3006,.F.);
#3958=ORIENTED_EDGE('',*,*,#3007,.F.);
#3959=ORIENTED_EDGE('',*,*,#3008,.T.);
#3960=ORIENTED_EDGE('',*,*,#3005,.T.);
#3961=ORIENTED_EDGE('',*,*,#3008,.F.);
#3962=ORIENTED_EDGE('',*,*,#3007,.T.);
#3963=ORIENTED_EDGE('',*,*,#3009,.T.);
#3964=ORIENTED_EDGE('',*,*,#3010,.T.);
#3965=ORIENTED_EDGE('',*,*,#3011,.T.);
#3966=ORIENTED_EDGE('',*,*,#3012,.F.);
#3967=ORIENTED_EDGE('',*,*,#3013,.T.);
#3968=ORIENTED_EDGE('',*,*,#3014,.T.);
#3969=ORIENTED_EDGE('',*,*,#3015,.T.);
#3970=ORIENTED_EDGE('',*,*,#3010,.F.);
#3971=ORIENTED_EDGE('',*,*,#3016,.T.);
#3972=ORIENTED_EDGE('',*,*,#3017,.T.);
#3973=ORIENTED_EDGE('',*,*,#3018,.T.);
#3974=ORIENTED_EDGE('',*,*,#3014,.F.);
#3975=ORIENTED_EDGE('',*,*,#3019,.T.);
#3976=ORIENTED_EDGE('',*,*,#3020,.T.);
#3977=ORIENTED_EDGE('',*,*,#3021,.T.);
#3978=ORIENTED_EDGE('',*,*,#3017,.F.);
#3979=ORIENTED_EDGE('',*,*,#3022,.T.);
#3980=ORIENTED_EDGE('',*,*,#3023,.T.);
#3981=ORIENTED_EDGE('',*,*,#3024,.T.);
#3982=ORIENTED_EDGE('',*,*,#3020,.F.);
#3983=ORIENTED_EDGE('',*,*,#3025,.T.);
#3984=ORIENTED_EDGE('',*,*,#3012,.T.);
#3985=ORIENTED_EDGE('',*,*,#3026,.T.);
#3986=ORIENTED_EDGE('',*,*,#3023,.F.);
#3987=ORIENTED_EDGE('',*,*,#3025,.F.);
#3988=ORIENTED_EDGE('',*,*,#3022,.F.);
#3989=ORIENTED_EDGE('',*,*,#3019,.F.);
#3990=ORIENTED_EDGE('',*,*,#3016,.F.);
#3991=ORIENTED_EDGE('',*,*,#3013,.F.);
#3992=ORIENTED_EDGE('',*,*,#3009,.F.);
#3993=ORIENTED_EDGE('',*,*,#3026,.F.);
#3994=ORIENTED_EDGE('',*,*,#3011,.F.);
#3995=ORIENTED_EDGE('',*,*,#3015,.F.);
#3996=ORIENTED_EDGE('',*,*,#3018,.F.);
#3997=ORIENTED_EDGE('',*,*,#3021,.F.);
#3998=ORIENTED_EDGE('',*,*,#3024,.F.);
#3999=ORIENTED_EDGE('',*,*,#3027,.F.);
#4000=ORIENTED_EDGE('',*,*,#3028,.F.);
#4001=ORIENTED_EDGE('',*,*,#3029,.T.);
#4002=ORIENTED_EDGE('',*,*,#3027,.T.);
#4003=ORIENTED_EDGE('',*,*,#3029,.F.);
#4004=ORIENTED_EDGE('',*,*,#3030,.F.);
#4005=ORIENTED_EDGE('',*,*,#3031,.T.);
#4006=ORIENTED_EDGE('',*,*,#3028,.T.);
#4007=ORIENTED_EDGE('',*,*,#3031,.F.);
#4008=ORIENTED_EDGE('',*,*,#3032,.F.);
#4009=ORIENTED_EDGE('',*,*,#3033,.T.);
#4010=ORIENTED_EDGE('',*,*,#3030,.T.);
#4011=ORIENTED_EDGE('',*,*,#3033,.F.);
#4012=ORIENTED_EDGE('',*,*,#3032,.T.);
#4013=ORIENTED_EDGE('',*,*,#3034,.F.);
#4014=ORIENTED_EDGE('',*,*,#3035,.F.);
#4015=ORIENTED_EDGE('',*,*,#3036,.T.);
#4016=ORIENTED_EDGE('',*,*,#3034,.T.);
#4017=ORIENTED_EDGE('',*,*,#3036,.F.);
#4018=ORIENTED_EDGE('',*,*,#3037,.F.);
#4019=ORIENTED_EDGE('',*,*,#3038,.T.);
#4020=ORIENTED_EDGE('',*,*,#3035,.T.);
#4021=ORIENTED_EDGE('',*,*,#3038,.F.);
#4022=ORIENTED_EDGE('',*,*,#3039,.F.);
#4023=ORIENTED_EDGE('',*,*,#3040,.T.);
#4024=ORIENTED_EDGE('',*,*,#3037,.T.);
#4025=ORIENTED_EDGE('',*,*,#3040,.F.);
#4026=ORIENTED_EDGE('',*,*,#3039,.T.);
#4027=ORIENTED_EDGE('',*,*,#3041,.T.);
#4028=ORIENTED_EDGE('',*,*,#3042,.T.);
#4029=ORIENTED_EDGE('',*,*,#3043,.T.);
#4030=ORIENTED_EDGE('',*,*,#3044,.F.);
#4031=ORIENTED_EDGE('',*,*,#3045,.T.);
#4032=ORIENTED_EDGE('',*,*,#3046,.T.);
#4033=ORIENTED_EDGE('',*,*,#3047,.T.);
#4034=ORIENTED_EDGE('',*,*,#3042,.F.);
#4035=ORIENTED_EDGE('',*,*,#3048,.T.);
#4036=ORIENTED_EDGE('',*,*,#3049,.T.);
#4037=ORIENTED_EDGE('',*,*,#3050,.T.);
#4038=ORIENTED_EDGE('',*,*,#3046,.F.);
#4039=ORIENTED_EDGE('',*,*,#3051,.T.);
#4040=ORIENTED_EDGE('',*,*,#3052,.T.);
#4041=ORIENTED_EDGE('',*,*,#3053,.T.);
#4042=ORIENTED_EDGE('',*,*,#3049,.F.);
#4043=ORIENTED_EDGE('',*,*,#3054,.T.);
#4044=ORIENTED_EDGE('',*,*,#3055,.T.);
#4045=ORIENTED_EDGE('',*,*,#3056,.T.);
#4046=ORIENTED_EDGE('',*,*,#3052,.F.);
#4047=ORIENTED_EDGE('',*,*,#3057,.T.);
#4048=ORIENTED_EDGE('',*,*,#3044,.T.);
#4049=ORIENTED_EDGE('',*,*,#3058,.T.);
#4050=ORIENTED_EDGE('',*,*,#3055,.F.);
#4051=ORIENTED_EDGE('',*,*,#3057,.F.);
#4052=ORIENTED_EDGE('',*,*,#3054,.F.);
#4053=ORIENTED_EDGE('',*,*,#3051,.F.);
#4054=ORIENTED_EDGE('',*,*,#3048,.F.);
#4055=ORIENTED_EDGE('',*,*,#3045,.F.);
#4056=ORIENTED_EDGE('',*,*,#3041,.F.);
#4057=ORIENTED_EDGE('',*,*,#3058,.F.);
#4058=ORIENTED_EDGE('',*,*,#3043,.F.);
#4059=ORIENTED_EDGE('',*,*,#3047,.F.);
#4060=ORIENTED_EDGE('',*,*,#3050,.F.);
#4061=ORIENTED_EDGE('',*,*,#3053,.F.);
#4062=ORIENTED_EDGE('',*,*,#3056,.F.);
#4063=ORIENTED_EDGE('',*,*,#3059,.F.);
#4064=ORIENTED_EDGE('',*,*,#3060,.T.);
#4065=ORIENTED_EDGE('',*,*,#3061,.F.);
#4066=ORIENTED_EDGE('',*,*,#3060,.F.);
#4067=ORIENTED_EDGE('',*,*,#3059,.T.);
#4068=ORIENTED_EDGE('',*,*,#3062,.F.);
#4069=ORIENTED_EDGE('',*,*,#3063,.F.);
#4070=ORIENTED_EDGE('',*,*,#3064,.F.);
#4071=ORIENTED_EDGE('',*,*,#3065,.T.);
#4072=ORIENTED_EDGE('',*,*,#3066,.F.);
#4073=ORIENTED_EDGE('',*,*,#3065,.F.);
#4074=ORIENTED_EDGE('',*,*,#3067,.F.);
#4075=ORIENTED_EDGE('',*,*,#3068,.F.);
#4076=ORIENTED_EDGE('',*,*,#3069,.F.);
#4077=ORIENTED_EDGE('',*,*,#3068,.T.);
#4078=ORIENTED_EDGE('',*,*,#3070,.T.);
#4079=ORIENTED_EDGE('',*,*,#3071,.F.);
#4080=ORIENTED_EDGE('',*,*,#3067,.T.);
#4081=ORIENTED_EDGE('',*,*,#3064,.T.);
#4082=ORIENTED_EDGE('',*,*,#3072,.F.);
#4083=ORIENTED_EDGE('',*,*,#3070,.F.);
#4084=ORIENTED_EDGE('',*,*,#3062,.T.);
#4085=ORIENTED_EDGE('',*,*,#3066,.T.);
#4086=ORIENTED_EDGE('',*,*,#3069,.T.);
#4087=ORIENTED_EDGE('',*,*,#3073,.F.);
#4088=ORIENTED_EDGE('',*,*,#3074,.T.);
#4089=ORIENTED_EDGE('',*,*,#3075,.T.);
#4090=ORIENTED_EDGE('',*,*,#3074,.F.);
#4091=ORIENTED_EDGE('',*,*,#3076,.F.);
#4092=ORIENTED_EDGE('',*,*,#3077,.T.);
#4093=ORIENTED_EDGE('',*,*,#3078,.T.);
#4094=ORIENTED_EDGE('',*,*,#3079,.T.);
#4095=ORIENTED_EDGE('',*,*,#3075,.F.);
#4096=ORIENTED_EDGE('',*,*,#3080,.F.);
#4097=ORIENTED_EDGE('',*,*,#3081,.F.);
#4098=ORIENTED_EDGE('',*,*,#3082,.F.);
#4099=ORIENTED_EDGE('',*,*,#3083,.F.);
#4100=ORIENTED_EDGE('',*,*,#3079,.F.);
#4101=ORIENTED_EDGE('',*,*,#3084,.T.);
#4102=ORIENTED_EDGE('',*,*,#3081,.T.);
#4103=ORIENTED_EDGE('',*,*,#3084,.F.);
#4104=ORIENTED_EDGE('',*,*,#3085,.T.);
#4105=ORIENTED_EDGE('',*,*,#3086,.T.);
#4106=ORIENTED_EDGE('',*,*,#3083,.T.);
#4107=ORIENTED_EDGE('',*,*,#3086,.F.);
#4108=ORIENTED_EDGE('',*,*,#3082,.T.);
#4109=ORIENTED_EDGE('',*,*,#3087,.T.);
#4110=ORIENTED_EDGE('',*,*,#3088,.T.);
#4111=ORIENTED_EDGE('',*,*,#3087,.F.);
#4112=ORIENTED_EDGE('',*,*,#3089,.F.);
#4113=ORIENTED_EDGE('',*,*,#3090,.T.);
#4114=ORIENTED_EDGE('',*,*,#3091,.T.);
#4115=ORIENTED_EDGE('',*,*,#3090,.F.);
#4116=ORIENTED_EDGE('',*,*,#3091,.F.);
#4117=ORIENTED_EDGE('',*,*,#3085,.F.);
#4118=ORIENTED_EDGE('',*,*,#3092,.F.);
#4119=ORIENTED_EDGE('',*,*,#3093,.F.);
#4120=ORIENTED_EDGE('',*,*,#3094,.T.);
#4121=ORIENTED_EDGE('',*,*,#3077,.F.);
#4122=ORIENTED_EDGE('',*,*,#3078,.F.);
#4123=ORIENTED_EDGE('',*,*,#3094,.F.);
#4124=ORIENTED_EDGE('',*,*,#3080,.T.);
#4125=ORIENTED_EDGE('',*,*,#3095,.T.);
#4126=ORIENTED_EDGE('',*,*,#3096,.T.);
#4127=ORIENTED_EDGE('',*,*,#3095,.F.);
#4128=ORIENTED_EDGE('',*,*,#3092,.T.);
#4129=ORIENTED_EDGE('',*,*,#3093,.T.);
#4130=ORIENTED_EDGE('',*,*,#3096,.F.);
#4131=ORIENTED_EDGE('',*,*,#3063,.T.);
#4132=ORIENTED_EDGE('',*,*,#3076,.T.);
#4133=ORIENTED_EDGE('',*,*,#3073,.T.);
#4134=ORIENTED_EDGE('',*,*,#3071,.T.);
#4135=ORIENTED_EDGE('',*,*,#3072,.T.);
#4136=ORIENTED_EDGE('',*,*,#3061,.T.);
#4137=ORIENTED_EDGE('',*,*,#3088,.F.);
#4138=ORIENTED_EDGE('',*,*,#3089,.T.);
#4139=ORIENTED_EDGE('',*,*,#3097,.F.);
#4140=ORIENTED_EDGE('',*,*,#3098,.T.);
#4141=ORIENTED_EDGE('',*,*,#3099,.T.);
#4142=ORIENTED_EDGE('',*,*,#3098,.F.);
#4143=ORIENTED_EDGE('',*,*,#3100,.F.);
#4144=ORIENTED_EDGE('',*,*,#3101,.T.);
#4145=ORIENTED_EDGE('',*,*,#3102,.T.);
#4146=ORIENTED_EDGE('',*,*,#3101,.F.);
#4147=ORIENTED_EDGE('',*,*,#3100,.T.);
#4148=ORIENTED_EDGE('',*,*,#3097,.T.);
#4149=ORIENTED_EDGE('',*,*,#3102,.F.);
#4150=ORIENTED_EDGE('',*,*,#3099,.F.);
#4151=ORIENTED_EDGE('',*,*,#3103,.F.);
#4152=ORIENTED_EDGE('',*,*,#3104,.T.);
#4153=ORIENTED_EDGE('',*,*,#3105,.F.);
#4154=ORIENTED_EDGE('',*,*,#3106,.F.);
#4155=ORIENTED_EDGE('',*,*,#3107,.T.);
#4156=ORIENTED_EDGE('',*,*,#3108,.F.);
#4157=ORIENTED_EDGE('',*,*,#3109,.F.);
#4158=ORIENTED_EDGE('',*,*,#3107,.F.);
#4159=ORIENTED_EDGE('',*,*,#3110,.F.);
#4160=ORIENTED_EDGE('',*,*,#3111,.F.);
#4161=ORIENTED_EDGE('',*,*,#3104,.F.);
#4162=ORIENTED_EDGE('',*,*,#3112,.F.);
#4163=ORIENTED_EDGE('',*,*,#3110,.T.);
#4164=ORIENTED_EDGE('',*,*,#3106,.T.);
#4165=ORIENTED_EDGE('',*,*,#3113,.F.);
#4166=ORIENTED_EDGE('',*,*,#3114,.T.);
#4167=ORIENTED_EDGE('',*,*,#3115,.T.);
#4168=ORIENTED_EDGE('',*,*,#3114,.F.);
#4169=ORIENTED_EDGE('',*,*,#3111,.T.);
#4170=ORIENTED_EDGE('',*,*,#3112,.T.);
#4171=ORIENTED_EDGE('',*,*,#3105,.T.);
#4172=ORIENTED_EDGE('',*,*,#3103,.T.);
#4173=ORIENTED_EDGE('',*,*,#3116,.F.);
#4174=ORIENTED_EDGE('',*,*,#3117,.T.);
#4175=ORIENTED_EDGE('',*,*,#3118,.T.);
#4176=ORIENTED_EDGE('',*,*,#3117,.F.);
#4177=ORIENTED_EDGE('',*,*,#3108,.T.);
#4178=ORIENTED_EDGE('',*,*,#3109,.T.);
#4179=ORIENTED_EDGE('',*,*,#3116,.T.);
#4180=ORIENTED_EDGE('',*,*,#3113,.T.);
#4181=ORIENTED_EDGE('',*,*,#3118,.F.);
#4182=ORIENTED_EDGE('',*,*,#3115,.F.);
#4183=ORIENTED_EDGE('',*,*,#3119,.F.);
#4184=ORIENTED_EDGE('',*,*,#3120,.T.);
#4185=ORIENTED_EDGE('',*,*,#3121,.F.);
#4186=ORIENTED_EDGE('',*,*,#3122,.F.);
#4187=ORIENTED_EDGE('',*,*,#3123,.F.);
#4188=ORIENTED_EDGE('',*,*,#3124,.T.);
#4189=ORIENTED_EDGE('',*,*,#3125,.F.);
#4190=ORIENTED_EDGE('',*,*,#3120,.F.);
#4191=ORIENTED_EDGE('',*,*,#3126,.F.);
#4192=ORIENTED_EDGE('',*,*,#3127,.F.);
#4193=ORIENTED_EDGE('',*,*,#3128,.F.);
#4194=ORIENTED_EDGE('',*,*,#3124,.F.);
#4195=ORIENTED_EDGE('',*,*,#3129,.T.);
#4196=ORIENTED_EDGE('',*,*,#3130,.T.);
#4197=ORIENTED_EDGE('',*,*,#3131,.T.);
#4198=ORIENTED_EDGE('',*,*,#3132,.T.);
#4199=ORIENTED_EDGE('',*,*,#3133,.T.);
#4200=ORIENTED_EDGE('',*,*,#3121,.T.);
#4201=ORIENTED_EDGE('',*,*,#3125,.T.);
#4202=ORIENTED_EDGE('',*,*,#3128,.T.);
#4203=ORIENTED_EDGE('',*,*,#3134,.T.);
#4204=ORIENTED_EDGE('',*,*,#3122,.T.);
#4205=ORIENTED_EDGE('',*,*,#3134,.F.);
#4206=ORIENTED_EDGE('',*,*,#3127,.T.);
#4207=ORIENTED_EDGE('',*,*,#3135,.T.);
#4208=ORIENTED_EDGE('',*,*,#3136,.F.);
#4209=ORIENTED_EDGE('',*,*,#3137,.T.);
#4210=ORIENTED_EDGE('',*,*,#3130,.F.);
#4211=ORIENTED_EDGE('',*,*,#3137,.F.);
#4212=ORIENTED_EDGE('',*,*,#3138,.F.);
#4213=ORIENTED_EDGE('',*,*,#3139,.T.);
#4214=ORIENTED_EDGE('',*,*,#3131,.F.);
#4215=ORIENTED_EDGE('',*,*,#3139,.F.);
#4216=ORIENTED_EDGE('',*,*,#3140,.F.);
#4217=ORIENTED_EDGE('',*,*,#3141,.T.);
#4218=ORIENTED_EDGE('',*,*,#3132,.F.);
#4219=ORIENTED_EDGE('',*,*,#3141,.F.);
#4220=ORIENTED_EDGE('',*,*,#3142,.F.);
#4221=ORIENTED_EDGE('',*,*,#3143,.T.);
#4222=ORIENTED_EDGE('',*,*,#3133,.F.);
#4223=ORIENTED_EDGE('',*,*,#3143,.F.);
#4224=ORIENTED_EDGE('',*,*,#3144,.F.);
#4225=ORIENTED_EDGE('',*,*,#3145,.F.);
#4226=ORIENTED_EDGE('',*,*,#3142,.T.);
#4227=ORIENTED_EDGE('',*,*,#3140,.T.);
#4228=ORIENTED_EDGE('',*,*,#3138,.T.);
#4229=ORIENTED_EDGE('',*,*,#3136,.T.);
#4230=ORIENTED_EDGE('',*,*,#3129,.F.);
#4231=ORIENTED_EDGE('',*,*,#3146,.T.);
#4232=ORIENTED_EDGE('',*,*,#3144,.T.);
#4233=ORIENTED_EDGE('',*,*,#3146,.F.);
#4234=ORIENTED_EDGE('',*,*,#3145,.T.);
#4235=ORIENTED_EDGE('',*,*,#3147,.T.);
#4236=ORIENTED_EDGE('',*,*,#3148,.T.);
#4237=ORIENTED_EDGE('',*,*,#3147,.F.);
#4238=ORIENTED_EDGE('',*,*,#3148,.F.);
#4239=ORIENTED_EDGE('',*,*,#3119,.T.);
#4240=ORIENTED_EDGE('',*,*,#3135,.F.);
#4241=ORIENTED_EDGE('',*,*,#3126,.T.);
#4242=ORIENTED_EDGE('',*,*,#3123,.T.);
#4243=ORIENTED_EDGE('',*,*,#3149,.F.);
#4244=ORIENTED_EDGE('',*,*,#3150,.T.);
#4245=ORIENTED_EDGE('',*,*,#3151,.T.);
#4246=ORIENTED_EDGE('',*,*,#3150,.F.);
#4247=ORIENTED_EDGE('',*,*,#3152,.F.);
#4248=ORIENTED_EDGE('',*,*,#3153,.T.);
#4249=ORIENTED_EDGE('',*,*,#3154,.T.);
#4250=ORIENTED_EDGE('',*,*,#3153,.F.);
#4251=ORIENTED_EDGE('',*,*,#3152,.T.);
#4252=ORIENTED_EDGE('',*,*,#3149,.T.);
#4253=ORIENTED_EDGE('',*,*,#3154,.F.);
#4254=ORIENTED_EDGE('',*,*,#3151,.F.);
#4255=ORIENTED_EDGE('',*,*,#3155,.T.);
#4256=ORIENTED_EDGE('',*,*,#3156,.T.);
#4257=ORIENTED_EDGE('',*,*,#3157,.T.);
#4258=ORIENTED_EDGE('',*,*,#3158,.T.);
#4259=ORIENTED_EDGE('',*,*,#3159,.T.);
#4260=ORIENTED_EDGE('',*,*,#3160,.T.);
#4261=ORIENTED_EDGE('',*,*,#3161,.F.);
#4262=ORIENTED_EDGE('',*,*,#3162,.T.);
#4263=ORIENTED_EDGE('',*,*,#3163,.T.);
#4264=ORIENTED_EDGE('',*,*,#3164,.T.);
#4265=ORIENTED_EDGE('',*,*,#3165,.T.);
#4266=ORIENTED_EDGE('',*,*,#3166,.T.);
#4267=ORIENTED_EDGE('',*,*,#3167,.T.);
#4268=ORIENTED_EDGE('',*,*,#3168,.F.);
#4269=ORIENTED_EDGE('',*,*,#3169,.F.);
#4270=ORIENTED_EDGE('',*,*,#3167,.F.);
#4271=ORIENTED_EDGE('',*,*,#3170,.F.);
#4272=ORIENTED_EDGE('',*,*,#3156,.F.);
#4273=ORIENTED_EDGE('',*,*,#3170,.T.);
#4274=ORIENTED_EDGE('',*,*,#3166,.F.);
#4275=ORIENTED_EDGE('',*,*,#3171,.F.);
#4276=ORIENTED_EDGE('',*,*,#3157,.F.);
#4277=ORIENTED_EDGE('',*,*,#3171,.T.);
#4278=ORIENTED_EDGE('',*,*,#3165,.F.);
#4279=ORIENTED_EDGE('',*,*,#3172,.F.);
#4280=ORIENTED_EDGE('',*,*,#3158,.F.);
#4281=ORIENTED_EDGE('',*,*,#3172,.T.);
#4282=ORIENTED_EDGE('',*,*,#3164,.F.);
#4283=ORIENTED_EDGE('',*,*,#3173,.F.);
#4284=ORIENTED_EDGE('',*,*,#3159,.F.);
#4285=ORIENTED_EDGE('',*,*,#3173,.T.);
#4286=ORIENTED_EDGE('',*,*,#3163,.F.);
#4287=ORIENTED_EDGE('',*,*,#3174,.F.);
#4288=ORIENTED_EDGE('',*,*,#3160,.F.);
#4289=ORIENTED_EDGE('',*,*,#3174,.T.);
#4290=ORIENTED_EDGE('',*,*,#3162,.F.);
#4291=ORIENTED_EDGE('',*,*,#3169,.T.);
#4292=ORIENTED_EDGE('',*,*,#3155,.F.);
#4293=ORIENTED_EDGE('',*,*,#3168,.T.);
#4294=ORIENTED_EDGE('',*,*,#3175,.T.);
#4295=ORIENTED_EDGE('',*,*,#3176,.T.);
#4296=ORIENTED_EDGE('',*,*,#3175,.F.);
#4297=ORIENTED_EDGE('',*,*,#3177,.F.);
#4298=ORIENTED_EDGE('',*,*,#3178,.T.);
#4299=ORIENTED_EDGE('',*,*,#3176,.F.);
#4300=ORIENTED_EDGE('',*,*,#3179,.T.);
#4301=ORIENTED_EDGE('',*,*,#3177,.T.);
#4302=ORIENTED_EDGE('',*,*,#3179,.F.);
#4303=ORIENTED_EDGE('',*,*,#3180,.F.);
#4304=ORIENTED_EDGE('',*,*,#3181,.T.);
#4305=ORIENTED_EDGE('',*,*,#3161,.T.);
#4306=ORIENTED_EDGE('',*,*,#3181,.F.);
#4307=ORIENTED_EDGE('',*,*,#3182,.F.);
#4308=ORIENTED_EDGE('',*,*,#3183,.T.);
#4309=ORIENTED_EDGE('',*,*,#3180,.T.);
#4310=ORIENTED_EDGE('',*,*,#3183,.F.);
#4311=ORIENTED_EDGE('',*,*,#3182,.T.);
#4312=ORIENTED_EDGE('',*,*,#3184,.F.);
#4313=ORIENTED_EDGE('',*,*,#3184,.T.);
#4314=ORIENTED_EDGE('',*,*,#3185,.T.);
#4315=ORIENTED_EDGE('',*,*,#3178,.F.);
#4316=ORIENTED_EDGE('',*,*,#3185,.F.);
#4317=ORIENTED_EDGE('',*,*,#3186,.F.);
#4318=ORIENTED_EDGE('',*,*,#3187,.T.);
#4319=ORIENTED_EDGE('',*,*,#3188,.T.);
#4320=ORIENTED_EDGE('',*,*,#3189,.F.);
#4321=ORIENTED_EDGE('',*,*,#3190,.F.);
#4322=ORIENTED_EDGE('',*,*,#3191,.T.);
#4323=ORIENTED_EDGE('',*,*,#3192,.T.);
#4324=ORIENTED_EDGE('',*,*,#3187,.F.);
#4325=ORIENTED_EDGE('',*,*,#3193,.F.);
#4326=ORIENTED_EDGE('',*,*,#3194,.T.);
#4327=ORIENTED_EDGE('',*,*,#3195,.T.);
#4328=ORIENTED_EDGE('',*,*,#3191,.F.);
#4329=ORIENTED_EDGE('',*,*,#3196,.F.);
#4330=ORIENTED_EDGE('',*,*,#3197,.T.);
#4331=ORIENTED_EDGE('',*,*,#3198,.T.);
#4332=ORIENTED_EDGE('',*,*,#3194,.F.);
#4333=ORIENTED_EDGE('',*,*,#3199,.F.);
#4334=ORIENTED_EDGE('',*,*,#3200,.T.);
#4335=ORIENTED_EDGE('',*,*,#3201,.T.);
#4336=ORIENTED_EDGE('',*,*,#3197,.F.);
#4337=ORIENTED_EDGE('',*,*,#3202,.F.);
#4338=ORIENTED_EDGE('',*,*,#3189,.T.);
#4339=ORIENTED_EDGE('',*,*,#3203,.T.);
#4340=ORIENTED_EDGE('',*,*,#3200,.F.);
#4341=ORIENTED_EDGE('',*,*,#3203,.F.);
#4342=ORIENTED_EDGE('',*,*,#3188,.F.);
#4343=ORIENTED_EDGE('',*,*,#3192,.F.);
#4344=ORIENTED_EDGE('',*,*,#3195,.F.);
#4345=ORIENTED_EDGE('',*,*,#3198,.F.);
#4346=ORIENTED_EDGE('',*,*,#3201,.F.);
#4347=ORIENTED_EDGE('',*,*,#3204,.F.);
#4348=ORIENTED_EDGE('',*,*,#3186,.T.);
#4349=ORIENTED_EDGE('',*,*,#3202,.T.);
#4350=ORIENTED_EDGE('',*,*,#3199,.T.);
#4351=ORIENTED_EDGE('',*,*,#3196,.T.);
#4352=ORIENTED_EDGE('',*,*,#3193,.T.);
#4353=ORIENTED_EDGE('',*,*,#3190,.T.);
#4354=ORIENTED_EDGE('',*,*,#3205,.F.);
#4355=ORIENTED_EDGE('',*,*,#3206,.T.);
#4356=ORIENTED_EDGE('',*,*,#3204,.T.);
#4357=ORIENTED_EDGE('',*,*,#3206,.F.);
#4358=ORIENTED_EDGE('',*,*,#3207,.F.);
#4359=ORIENTED_EDGE('',*,*,#3208,.T.);
#4360=ORIENTED_EDGE('',*,*,#3205,.T.);
#4361=ORIENTED_EDGE('',*,*,#3208,.F.);
#4362=ORIENTED_EDGE('',*,*,#3209,.F.);
#4363=ORIENTED_EDGE('',*,*,#3210,.T.);
#4364=ORIENTED_EDGE('',*,*,#3207,.T.);
#4365=ORIENTED_EDGE('',*,*,#3210,.F.);
#4366=ORIENTED_EDGE('',*,*,#3209,.T.);
#4367=ORIENTED_EDGE('',*,*,#3211,.F.);
#4368=ORIENTED_EDGE('',*,*,#3212,.F.);
#4369=ORIENTED_EDGE('',*,*,#3213,.F.);
#4370=ORIENTED_EDGE('',*,*,#3214,.F.);
#4371=ORIENTED_EDGE('',*,*,#3215,.F.);
#4372=ORIENTED_EDGE('',*,*,#3216,.F.);
#4373=ORIENTED_EDGE('',*,*,#3217,.F.);
#4374=ORIENTED_EDGE('',*,*,#3218,.F.);
#4375=ORIENTED_EDGE('',*,*,#3215,.T.);
#4376=ORIENTED_EDGE('',*,*,#3219,.T.);
#4377=ORIENTED_EDGE('',*,*,#3220,.T.);
#4378=ORIENTED_EDGE('',*,*,#3221,.T.);
#4379=ORIENTED_EDGE('',*,*,#3214,.T.);
#4380=ORIENTED_EDGE('',*,*,#3222,.F.);
#4381=ORIENTED_EDGE('',*,*,#3223,.T.);
#4382=ORIENTED_EDGE('',*,*,#3219,.F.);
#4383=ORIENTED_EDGE('',*,*,#3213,.T.);
#4384=ORIENTED_EDGE('',*,*,#3224,.T.);
#4385=ORIENTED_EDGE('',*,*,#3225,.T.);
#4386=ORIENTED_EDGE('',*,*,#3222,.T.);
#4387=ORIENTED_EDGE('',*,*,#3212,.T.);
#4388=ORIENTED_EDGE('',*,*,#3226,.F.);
#4389=ORIENTED_EDGE('',*,*,#3227,.T.);
#4390=ORIENTED_EDGE('',*,*,#3224,.F.);
#4391=ORIENTED_EDGE('',*,*,#3228,.F.);
#4392=ORIENTED_EDGE('',*,*,#3229,.F.);
#4393=ORIENTED_EDGE('',*,*,#3220,.F.);
#4394=ORIENTED_EDGE('',*,*,#3223,.F.);
#4395=ORIENTED_EDGE('',*,*,#3225,.F.);
#4396=ORIENTED_EDGE('',*,*,#3227,.F.);
#4397=ORIENTED_EDGE('',*,*,#3230,.F.);
#4398=ORIENTED_EDGE('',*,*,#3231,.F.);
#4399=ORIENTED_EDGE('',*,*,#3216,.T.);
#4400=ORIENTED_EDGE('',*,*,#3221,.F.);
#4401=ORIENTED_EDGE('',*,*,#3229,.T.);
#4402=ORIENTED_EDGE('',*,*,#3232,.F.);
#4403=ORIENTED_EDGE('',*,*,#3211,.T.);
#4404=ORIENTED_EDGE('',*,*,#3233,.T.);
#4405=ORIENTED_EDGE('',*,*,#3230,.T.);
#4406=ORIENTED_EDGE('',*,*,#3226,.T.);
#4407=ORIENTED_EDGE('',*,*,#3217,.T.);
#4408=ORIENTED_EDGE('',*,*,#3232,.T.);
#4409=ORIENTED_EDGE('',*,*,#3228,.T.);
#4410=ORIENTED_EDGE('',*,*,#3234,.T.);
#4411=ORIENTED_EDGE('',*,*,#3218,.T.);
#4412=ORIENTED_EDGE('',*,*,#3234,.F.);
#4413=ORIENTED_EDGE('',*,*,#3231,.T.);
#4414=ORIENTED_EDGE('',*,*,#3233,.F.);
#4415=ORIENTED_EDGE('',*,*,#3235,.F.);
#4416=ORIENTED_EDGE('',*,*,#3236,.F.);
#4417=ORIENTED_EDGE('',*,*,#3237,.T.);
#4418=ORIENTED_EDGE('',*,*,#3235,.T.);
#4419=ORIENTED_EDGE('',*,*,#3237,.F.);
#4420=ORIENTED_EDGE('',*,*,#3238,.F.);
#4421=ORIENTED_EDGE('',*,*,#3239,.T.);
#4422=ORIENTED_EDGE('',*,*,#3236,.T.);
#4423=ORIENTED_EDGE('',*,*,#3239,.F.);
#4424=ORIENTED_EDGE('',*,*,#3240,.F.);
#4425=ORIENTED_EDGE('',*,*,#3241,.T.);
#4426=ORIENTED_EDGE('',*,*,#3238,.T.);
#4427=ORIENTED_EDGE('',*,*,#3241,.F.);
#4428=ORIENTED_EDGE('',*,*,#3240,.T.);
#4429=ORIENTED_EDGE('',*,*,#3242,.F.);
#4430=ORIENTED_EDGE('',*,*,#3243,.F.);
#4431=ORIENTED_EDGE('',*,*,#3244,.T.);
#4432=ORIENTED_EDGE('',*,*,#3242,.T.);
#4433=ORIENTED_EDGE('',*,*,#3244,.F.);
#4434=ORIENTED_EDGE('',*,*,#3245,.F.);
#4435=ORIENTED_EDGE('',*,*,#3246,.T.);
#4436=ORIENTED_EDGE('',*,*,#3243,.T.);
#4437=ORIENTED_EDGE('',*,*,#3246,.F.);
#4438=ORIENTED_EDGE('',*,*,#3247,.F.);
#4439=ORIENTED_EDGE('',*,*,#3248,.T.);
#4440=ORIENTED_EDGE('',*,*,#3245,.T.);
#4441=ORIENTED_EDGE('',*,*,#3248,.F.);
#4442=ORIENTED_EDGE('',*,*,#3247,.T.);
#4443=ORIENTED_EDGE('',*,*,#3249,.T.);
#4444=ORIENTED_EDGE('',*,*,#3250,.T.);
#4445=ORIENTED_EDGE('',*,*,#3251,.T.);
#4446=ORIENTED_EDGE('',*,*,#3252,.F.);
#4447=ORIENTED_EDGE('',*,*,#3253,.T.);
#4448=ORIENTED_EDGE('',*,*,#3254,.T.);
#4449=ORIENTED_EDGE('',*,*,#3255,.T.);
#4450=ORIENTED_EDGE('',*,*,#3250,.F.);
#4451=ORIENTED_EDGE('',*,*,#3256,.T.);
#4452=ORIENTED_EDGE('',*,*,#3257,.T.);
#4453=ORIENTED_EDGE('',*,*,#3258,.T.);
#4454=ORIENTED_EDGE('',*,*,#3254,.F.);
#4455=ORIENTED_EDGE('',*,*,#3259,.T.);
#4456=ORIENTED_EDGE('',*,*,#3260,.T.);
#4457=ORIENTED_EDGE('',*,*,#3261,.T.);
#4458=ORIENTED_EDGE('',*,*,#3257,.F.);
#4459=ORIENTED_EDGE('',*,*,#3262,.T.);
#4460=ORIENTED_EDGE('',*,*,#3263,.T.);
#4461=ORIENTED_EDGE('',*,*,#3264,.T.);
#4462=ORIENTED_EDGE('',*,*,#3260,.F.);
#4463=ORIENTED_EDGE('',*,*,#3265,.T.);
#4464=ORIENTED_EDGE('',*,*,#3252,.T.);
#4465=ORIENTED_EDGE('',*,*,#3266,.T.);
#4466=ORIENTED_EDGE('',*,*,#3263,.F.);
#4467=ORIENTED_EDGE('',*,*,#3265,.F.);
#4468=ORIENTED_EDGE('',*,*,#3262,.F.);
#4469=ORIENTED_EDGE('',*,*,#3259,.F.);
#4470=ORIENTED_EDGE('',*,*,#3256,.F.);
#4471=ORIENTED_EDGE('',*,*,#3253,.F.);
#4472=ORIENTED_EDGE('',*,*,#3249,.F.);
#4473=ORIENTED_EDGE('',*,*,#3266,.F.);
#4474=ORIENTED_EDGE('',*,*,#3251,.F.);
#4475=ORIENTED_EDGE('',*,*,#3255,.F.);
#4476=ORIENTED_EDGE('',*,*,#3258,.F.);
#4477=ORIENTED_EDGE('',*,*,#3261,.F.);
#4478=ORIENTED_EDGE('',*,*,#3264,.F.);
#4479=CYLINDRICAL_SURFACE('',#5207,0.25);
#4480=CYLINDRICAL_SURFACE('',#5210,0.25);
#4481=CYLINDRICAL_SURFACE('',#5213,0.25);
#4482=CYLINDRICAL_SURFACE('',#5216,0.25);
#4483=CYLINDRICAL_SURFACE('',#5226,0.165);
#4484=CYLINDRICAL_SURFACE('',#5230,0.165);
#4485=CYLINDRICAL_SURFACE('',#5234,0.165);
#4486=CYLINDRICAL_SURFACE('',#5238,0.165);
#4487=CYLINDRICAL_SURFACE('',#5242,0.165);
#4488=CYLINDRICAL_SURFACE('',#5246,0.165);
#4489=CYLINDRICAL_SURFACE('',#5250,0.165);
#4490=CYLINDRICAL_SURFACE('',#5254,0.165);
#4491=CYLINDRICAL_SURFACE('',#5258,0.685);
#4492=CYLINDRICAL_SURFACE('',#5259,0.33);
#4493=CYLINDRICAL_SURFACE('',#5262,0.33);
#4494=CYLINDRICAL_SURFACE('',#5265,0.33);
#4495=CYLINDRICAL_SURFACE('',#5268,0.33);
#4496=CYLINDRICAL_SURFACE('',#5297,2.35);
#4497=CYLINDRICAL_SURFACE('',#5300,3.5);
#4498=CYLINDRICAL_SURFACE('',#5306,1.16);
#4499=CYLINDRICAL_SURFACE('',#5313,1.005);
#4500=CYLINDRICAL_SURFACE('',#5315,1.005);
#4501=CYLINDRICAL_SURFACE('',#5317,2.34);
#4502=CYLINDRICAL_SURFACE('',#5327,1.16);
#4503=CYLINDRICAL_SURFACE('',#5334,1.005);
#4504=CYLINDRICAL_SURFACE('',#5336,1.005);
#4505=CYLINDRICAL_SURFACE('',#5338,2.34);
#4506=CYLINDRICAL_SURFACE('',#5348,0.685);
#4507=CYLINDRICAL_SURFACE('',#5350,0.685);
#4508=CYLINDRICAL_SURFACE('',#5357,2.34);
#4509=CYLINDRICAL_SURFACE('',#5359,0.46);
#4510=CYLINDRICAL_SURFACE('',#5360,1.2);
#4511=CYLINDRICAL_SURFACE('',#5364,0.225);
#4512=CYLINDRICAL_SURFACE('',#5367,0.225);
#4513=CYLINDRICAL_SURFACE('',#5370,0.225);
#4514=CYLINDRICAL_SURFACE('',#5373,0.225);
#4515=CYLINDRICAL_SURFACE('',#5376,2.34);
#4516=CYLINDRICAL_SURFACE('',#5381,1.8);
#4517=CYLINDRICAL_SURFACE('',#5383,3.5);
#4518=CYLINDRICAL_SURFACE('',#5389,0.225);
#4519=CYLINDRICAL_SURFACE('',#5392,0.225);
#4520=CYLINDRICAL_SURFACE('',#5395,0.225);
#4521=CYLINDRICAL_SURFACE('',#5398,0.225);
#4522=CYLINDRICAL_SURFACE('',#5401,2.34);
#4523=CYLINDRICAL_SURFACE('',#5406,1.8);
#4524=CYLINDRICAL_SURFACE('',#5408,3.5);
#4525=CYLINDRICAL_SURFACE('',#5435,1.63531);
#4526=CYLINDRICAL_SURFACE('',#5437,1.);
#4527=CYLINDRICAL_SURFACE('',#5443,1.63531);
#4528=CYLINDRICAL_SURFACE('',#5455,1.71469);
#4529=CYLINDRICAL_SURFACE('',#5462,2.35);
#4530=CYLINDRICAL_SURFACE('',#5467,1.71469);
#4531=CYLINDRICAL_SURFACE('',#5489,1.706752);
#4532=CYLINDRICAL_SURFACE('',#5529,1.643248);
#4533=CYLINDRICAL_SURFACE('',#5543,1.70469);
#4534=CYLINDRICAL_SURFACE('',#5547,1.65031);
#4535=CYLINDRICAL_SURFACE('',#5551,1.70469);
#4536=CYLINDRICAL_SURFACE('',#5555,1.65031);
#4537=CYLINDRICAL_SURFACE('',#5566,0.5);
#4538=CYLINDRICAL_SURFACE('',#5574,0.2942);
#4539=CYLINDRICAL_SURFACE('',#5592,0.35);
#4540=CYLINDRICAL_SURFACE('',#5600,0.1954);
#4541=CYLINDRICAL_SURFACE('',#5615,0.21);
#4542=CYLINDRICAL_SURFACE('',#5624,1.);
#4543=CYLINDRICAL_SURFACE('',#5637,1.2);
#4544=CYLINDRICAL_SURFACE('',#5638,0.4);
#4545=CYLINDRICAL_SURFACE('',#5640,1.);
#4546=CYLINDRICAL_SURFACE('',#5642,0.685);
#4547=CYLINDRICAL_SURFACE('',#5646,0.3);
#4548=CYLINDRICAL_SURFACE('',#5647,0.4);
#4549=CYLINDRICAL_SURFACE('',#5653,1.005);
#4550=CYLINDRICAL_SURFACE('',#5656,1.35);
#4551=CYLINDRICAL_SURFACE('',#5664,0.21);
#4552=CYLINDRICAL_SURFACE('',#5668,1.005);
#4553=CYLINDRICAL_SURFACE('',#5671,1.5);
#4554=CYLINDRICAL_SURFACE('',#5687,1.);
#4555=CYLINDRICAL_SURFACE('',#5689,0.275);
#4556=CYLINDRICAL_SURFACE('',#5691,0.275);
#4557=CYLINDRICAL_SURFACE('',#5693,0.275);
#4558=CYLINDRICAL_SURFACE('',#5695,0.275);
#4559=CYLINDRICAL_SURFACE('',#5700,3.);
#4560=CYLINDRICAL_SURFACE('',#5701,1.6);
#4561=CYLINDRICAL_SURFACE('',#5705,0.275);
#4562=CYLINDRICAL_SURFACE('',#5708,1.2);
#4563=CYLINDRICAL_SURFACE('',#5724,0.685);
#4564=CYLINDRICAL_SURFACE('',#5730,0.685);
#4565=CYLINDRICAL_SURFACE('',#5736,0.46);
#4566=CYLINDRICAL_SURFACE('',#5775,0.24505);
#4567=CYLINDRICAL_SURFACE('',#5796,0.425);
#4568=CYLINDRICAL_SURFACE('',#5804,0.24505);
#4569=ADVANCED_FACE('',(#656),#4479,.F.);
#4570=ADVANCED_FACE('',(#657),#4480,.F.);
#4571=ADVANCED_FACE('',(#658),#4481,.F.);
#4572=ADVANCED_FACE('',(#659),#4482,.F.);
#4573=ADVANCED_FACE('',(#660),#487,.T.);
#4574=ADVANCED_FACE('',(#661),#488,.T.);
#4575=ADVANCED_FACE('',(#662),#489,.T.);
#4576=ADVANCED_FACE('',(#663),#490,.T.);
#4577=ADVANCED_FACE('',(#664,#380,#381,#382,#383),#491,.T.);
#4578=ADVANCED_FACE('',(#665,#384,#385,#386,#387),#492,.F.);
#4579=ADVANCED_FACE('',(#666),#4483,.F.);
#4580=ADVANCED_FACE('',(#667),#493,.T.);
#4581=ADVANCED_FACE('',(#668),#4484,.F.);
#4582=ADVANCED_FACE('',(#669),#494,.T.);
#4583=ADVANCED_FACE('',(#670),#4485,.F.);
#4584=ADVANCED_FACE('',(#671),#495,.T.);
#4585=ADVANCED_FACE('',(#672),#4486,.F.);
#4586=ADVANCED_FACE('',(#673),#496,.T.);
#4587=ADVANCED_FACE('',(#674),#4487,.F.);
#4588=ADVANCED_FACE('',(#675),#497,.F.);
#4589=ADVANCED_FACE('',(#676),#4488,.F.);
#4590=ADVANCED_FACE('',(#677),#498,.F.);
#4591=ADVANCED_FACE('',(#678),#4489,.F.);
#4592=ADVANCED_FACE('',(#679),#499,.F.);
#4593=ADVANCED_FACE('',(#680),#4490,.F.);
#4594=ADVANCED_FACE('',(#681),#500,.F.);
#4595=ADVANCED_FACE('',(#682),#4491,.F.);
#4596=ADVANCED_FACE('',(#683),#4492,.F.);
#4597=ADVANCED_FACE('',(#684),#4493,.F.);
#4598=ADVANCED_FACE('',(#685),#4494,.F.);
#4599=ADVANCED_FACE('',(#686),#4495,.F.);
#4600=ADVANCED_FACE('',(#687),#501,.T.);
#4601=ADVANCED_FACE('',(#688),#502,.T.);
#4602=ADVANCED_FACE('',(#689),#503,.F.);
#4603=ADVANCED_FACE('',(#690),#504,.F.);
#4604=ADVANCED_FACE('',(#691,#388),#505,.T.);
#4605=ADVANCED_FACE('',(#692,#389),#506,.T.);
#4606=ADVANCED_FACE('',(#693),#507,.T.);
#4607=ADVANCED_FACE('',(#694,#390,#391),#508,.T.);
#4608=ADVANCED_FACE('',(#695),#509,.T.);
#4609=ADVANCED_FACE('',(#696),#510,.T.);
#4610=ADVANCED_FACE('',(#697),#511,.T.);
#4611=ADVANCED_FACE('',(#698),#512,.F.);
#4612=ADVANCED_FACE('',(#699),#513,.F.);
#4613=ADVANCED_FACE('',(#700,#392),#514,.T.);
#4614=ADVANCED_FACE('',(#701,#393),#515,.T.);
#4615=ADVANCED_FACE('',(#702),#516,.T.);
#4616=ADVANCED_FACE('',(#703,#394,#395),#517,.T.);
#4617=ADVANCED_FACE('',(#704),#518,.T.);
#4618=ADVANCED_FACE('',(#705,#396),#4496,.F.);
#4619=ADVANCED_FACE('',(#706,#397,#398,#399),#4497,.T.);
#4620=ADVANCED_FACE('',(#707,#400,#401,#402,#403,#404),#519,.T.);
#4621=ADVANCED_FACE('',(#708,#405,#406,#407,#408,#409),#520,.F.);
#4622=ADVANCED_FACE('',(#709),#4498,.F.);
#4623=ADVANCED_FACE('',(#710,#410),#521,.F.);
#4624=ADVANCED_FACE('',(#711,#411),#522,.T.);
#4625=ADVANCED_FACE('',(#712),#4499,.F.);
#4626=ADVANCED_FACE('',(#713),#4500,.F.);
#4627=ADVANCED_FACE('',(#714),#4501,.T.);
#4628=ADVANCED_FACE('',(#715,#412),#523,.T.);
#4629=ADVANCED_FACE('',(#716,#413),#524,.F.);
#4630=ADVANCED_FACE('',(#717),#221,.T.);
#4631=ADVANCED_FACE('',(#718),#4502,.F.);
#4632=ADVANCED_FACE('',(#719,#414),#525,.F.);
#4633=ADVANCED_FACE('',(#720,#415),#526,.T.);
#4634=ADVANCED_FACE('',(#721),#4503,.F.);
#4635=ADVANCED_FACE('',(#722),#4504,.F.);
#4636=ADVANCED_FACE('',(#723),#4505,.T.);
#4637=ADVANCED_FACE('',(#724,#416),#527,.T.);
#4638=ADVANCED_FACE('',(#725,#417),#528,.F.);
#4639=ADVANCED_FACE('',(#726),#222,.T.);
#4640=ADVANCED_FACE('',(#727),#4506,.F.);
#4641=ADVANCED_FACE('',(#728),#4507,.F.);
#4642=ADVANCED_FACE('',(#729,#418),#529,.T.);
#4643=ADVANCED_FACE('',(#730,#419),#530,.T.);
#4644=ADVANCED_FACE('',(#731),#4508,.T.);
#4645=ADVANCED_FACE('',(#732),#4509,.F.);
#4646=ADVANCED_FACE('',(#733,#420),#4510,.F.);
#4647=ADVANCED_FACE('',(#734,#421),#531,.F.);
#4648=ADVANCED_FACE('',(#735),#4511,.F.);
#4649=ADVANCED_FACE('',(#736),#4512,.F.);
#4650=ADVANCED_FACE('',(#737),#4513,.F.);
#4651=ADVANCED_FACE('',(#738),#4514,.F.);
#4652=ADVANCED_FACE('',(#739),#4515,.T.);
#4653=ADVANCED_FACE('',(#740,#422),#532,.T.);
#4654=ADVANCED_FACE('',(#741),#4516,.F.);
#4655=ADVANCED_FACE('',(#742),#4517,.T.);
#4656=ADVANCED_FACE('',(#743,#423,#424,#425,#426,#427),#533,.T.);
#4657=ADVANCED_FACE('',(#744,#428,#429,#430,#431,#432),#534,.F.);
#4658=ADVANCED_FACE('',(#745),#4518,.F.);
#4659=ADVANCED_FACE('',(#746),#4519,.F.);
#4660=ADVANCED_FACE('',(#747),#4520,.F.);
#4661=ADVANCED_FACE('',(#748),#4521,.F.);
#4662=ADVANCED_FACE('',(#749),#4522,.T.);
#4663=ADVANCED_FACE('',(#750,#433),#535,.F.);
#4664=ADVANCED_FACE('',(#751),#4523,.F.);
#4665=ADVANCED_FACE('',(#752),#4524,.T.);
#4666=ADVANCED_FACE('',(#753,#434,#435,#436,#437,#438),#536,.T.);
#4667=ADVANCED_FACE('',(#754,#439,#440,#441,#442,#443),#537,.F.);
#4668=ADVANCED_FACE('',(#755),#538,.T.);
#4669=ADVANCED_FACE('',(#756),#539,.T.);
#4670=ADVANCED_FACE('',(#757),#540,.T.);
#4671=ADVANCED_FACE('',(#758),#541,.T.);
#4672=ADVANCED_FACE('',(#759),#542,.T.);
#4673=ADVANCED_FACE('',(#760),#543,.F.);
#4674=ADVANCED_FACE('',(#761),#544,.T.);
#4675=ADVANCED_FACE('',(#762),#545,.T.);
#4676=ADVANCED_FACE('',(#763),#546,.T.);
#4677=ADVANCED_FACE('',(#764),#547,.T.);
#4678=ADVANCED_FACE('',(#765),#548,.T.);
#4679=ADVANCED_FACE('',(#766),#549,.F.);
#4680=ADVANCED_FACE('',(#767),#223,.F.);
#4681=ADVANCED_FACE('',(#768),#4525,.T.);
#4682=ADVANCED_FACE('',(#769),#4526,.F.);
#4683=ADVANCED_FACE('',(#770),#201,.F.);
#4684=ADVANCED_FACE('',(#771,#444),#550,.T.);
#4685=ADVANCED_FACE('',(#772),#4527,.T.);
#4686=ADVANCED_FACE('',(#773,#445),#551,.T.);
#4687=ADVANCED_FACE('',(#774),#202,.F.);
#4688=ADVANCED_FACE('',(#775),#224,.F.);
#4689=ADVANCED_FACE('',(#776),#4528,.F.);
#4690=ADVANCED_FACE('',(#777,#446),#552,.T.);
#4691=ADVANCED_FACE('',(#778),#203,.T.);
#4692=ADVANCED_FACE('',(#779),#4529,.T.);
#4693=ADVANCED_FACE('',(#780),#204,.T.);
#4694=ADVANCED_FACE('',(#781,#447),#553,.T.);
#4695=ADVANCED_FACE('',(#782),#4530,.F.);
#4696=ADVANCED_FACE('',(#783),#185,.T.);
#4697=ADVANCED_FACE('',(#784),#186,.T.);
#4698=ADVANCED_FACE('',(#785),#187,.T.);
#4699=ADVANCED_FACE('',(#786),#188,.T.);
#4700=ADVANCED_FACE('',(#787),#189,.T.);
#4701=ADVANCED_FACE('',(#788),#190,.T.);
#4702=ADVANCED_FACE('',(#789),#191,.T.);
#4703=ADVANCED_FACE('',(#790),#192,.T.);
#4704=ADVANCED_FACE('',(#791),#193,.F.);
#4705=ADVANCED_FACE('',(#792),#4531,.T.);
#4706=ADVANCED_FACE('',(#793),#554,.T.);
#4707=ADVANCED_FACE('',(#794),#194,.F.);
#4708=ADVANCED_FACE('',(#795),#555,.T.);
#4709=ADVANCED_FACE('',(#796),#195,.F.);
#4710=ADVANCED_FACE('',(#797),#556,.T.);
#4711=ADVANCED_FACE('',(#798),#196,.F.);
#4712=ADVANCED_FACE('',(#799),#557,.T.);
#4713=ADVANCED_FACE('',(#800),#197,.F.);
#4714=ADVANCED_FACE('',(#801),#558,.T.);
#4715=ADVANCED_FACE('',(#802),#198,.F.);
#4716=ADVANCED_FACE('',(#803),#559,.T.);
#4717=ADVANCED_FACE('',(#804),#199,.F.);
#4718=ADVANCED_FACE('',(#805),#4532,.F.);
#4719=ADVANCED_FACE('',(#806),#560,.T.);
#4720=ADVANCED_FACE('',(#807),#200,.F.);
#4721=ADVANCED_FACE('',(#808,#448),#561,.T.);
#4722=ADVANCED_FACE('',(#809),#562,.T.);
#4723=ADVANCED_FACE('',(#810,#449),#563,.T.);
#4724=ADVANCED_FACE('',(#811),#4533,.T.);
#4725=ADVANCED_FACE('',(#812,#450),#564,.T.);
#4726=ADVANCED_FACE('',(#813),#4534,.F.);
#4727=ADVANCED_FACE('',(#814,#451),#565,.T.);
#4728=ADVANCED_FACE('',(#815),#4535,.T.);
#4729=ADVANCED_FACE('',(#816,#452),#566,.T.);
#4730=ADVANCED_FACE('',(#817),#4536,.F.);
#4731=ADVANCED_FACE('',(#818),#567,.T.);
#4732=ADVANCED_FACE('',(#819),#205,.T.);
#4733=ADVANCED_FACE('',(#820),#4537,.T.);
#4734=ADVANCED_FACE('',(#821),#206,.T.);
#4735=ADVANCED_FACE('',(#822,#453),#568,.T.);
#4736=ADVANCED_FACE('',(#823),#207,.T.);
#4737=ADVANCED_FACE('',(#824),#4538,.T.);
#4738=ADVANCED_FACE('',(#825),#208,.T.);
#4739=ADVANCED_FACE('',(#826),#569,.T.);
#4740=ADVANCED_FACE('',(#827),#570,.F.);
#4741=ADVANCED_FACE('',(#828),#571,.F.);
#4742=ADVANCED_FACE('',(#829),#572,.F.);
#4743=ADVANCED_FACE('',(#830),#573,.F.);
#4744=ADVANCED_FACE('',(#831),#574,.F.);
#4745=ADVANCED_FACE('',(#832),#575,.F.);
#4746=ADVANCED_FACE('',(#833),#576,.F.);
#4747=ADVANCED_FACE('',(#834),#577,.F.);
#4748=ADVANCED_FACE('',(#835),#578,.T.);
#4749=ADVANCED_FACE('',(#836),#209,.T.);
#4750=ADVANCED_FACE('',(#837),#4539,.T.);
#4751=ADVANCED_FACE('',(#838),#210,.T.);
#4752=ADVANCED_FACE('',(#839,#454),#579,.T.);
#4753=ADVANCED_FACE('',(#840),#211,.T.);
#4754=ADVANCED_FACE('',(#841),#4540,.T.);
#4755=ADVANCED_FACE('',(#842),#212,.T.);
#4756=ADVANCED_FACE('',(#843),#580,.T.);
#4757=ADVANCED_FACE('',(#844),#581,.F.);
#4758=ADVANCED_FACE('',(#845),#582,.F.);
#4759=ADVANCED_FACE('',(#846),#583,.F.);
#4760=ADVANCED_FACE('',(#847),#584,.F.);
#4761=ADVANCED_FACE('',(#848),#585,.F.);
#4762=ADVANCED_FACE('',(#849),#586,.F.);
#4763=ADVANCED_FACE('',(#850),#587,.F.);
#4764=ADVANCED_FACE('',(#851),#588,.F.);
#4765=ADVANCED_FACE('',(#852),#4541,.F.);
#4766=ADVANCED_FACE('',(#853),#589,.T.);
#4767=ADVANCED_FACE('',(#854),#590,.F.);
#4768=ADVANCED_FACE('',(#855),#591,.T.);
#4769=ADVANCED_FACE('',(#856),#592,.F.);
#4770=ADVANCED_FACE('',(#857),#593,.F.);
#4771=ADVANCED_FACE('',(#858,#455),#4542,.T.);
#4772=ADVANCED_FACE('',(#859,#456),#594,.T.);
#4773=ADVANCED_FACE('',(#860),#595,.T.);
#4774=ADVANCED_FACE('',(#861,#457),#596,.F.);
#4775=ADVANCED_FACE('',(#862),#597,.F.);
#4776=ADVANCED_FACE('',(#863),#4543,.T.);
#4777=ADVANCED_FACE('',(#864),#4544,.F.);
#4778=ADVANCED_FACE('',(#865),#4545,.T.);
#4779=ADVANCED_FACE('',(#866),#4546,.F.);
#4780=ADVANCED_FACE('',(#867,#458),#598,.F.);
#4781=ADVANCED_FACE('',(#868),#4547,.F.);
#4782=ADVANCED_FACE('',(#869,#459),#4548,.F.);
#4783=ADVANCED_FACE('',(#870),#599,.F.);
#4784=ADVANCED_FACE('',(#871,#460),#600,.T.);
#4785=ADVANCED_FACE('',(#872,#461),#601,.F.);
#4786=ADVANCED_FACE('',(#873),#4549,.F.);
#4787=ADVANCED_FACE('',(#874),#4550,.T.);
#4788=ADVANCED_FACE('',(#875,#462),#602,.T.);
#4789=ADVANCED_FACE('',(#876,#463),#603,.F.);
#4790=ADVANCED_FACE('',(#877),#604,.T.);
#4791=ADVANCED_FACE('',(#878),#4551,.F.);
#4792=ADVANCED_FACE('',(#879),#605,.T.);
#4793=ADVANCED_FACE('',(#880,#464),#4552,.F.);
#4794=ADVANCED_FACE('',(#881,#465),#4553,.T.);
#4795=ADVANCED_FACE('',(#882,#466),#606,.T.);
#4796=ADVANCED_FACE('',(#883,#467),#607,.F.);
#4797=ADVANCED_FACE('',(#884),#608,.F.);
#4798=ADVANCED_FACE('',(#885),#609,.F.);
#4799=ADVANCED_FACE('',(#886),#610,.F.);
#4800=ADVANCED_FACE('',(#887,#468,#469,#470,#471,#472),#611,.T.);
#4801=ADVANCED_FACE('',(#888),#4554,.F.);
#4802=ADVANCED_FACE('',(#889),#4555,.F.);
#4803=ADVANCED_FACE('',(#890),#4556,.F.);
#4804=ADVANCED_FACE('',(#891),#4557,.F.);
#4805=ADVANCED_FACE('',(#892),#4558,.F.);
#4806=ADVANCED_FACE('',(#893,#473,#474,#475,#476,#477),#612,.F.);
#4807=ADVANCED_FACE('',(#894),#4559,.T.);
#4808=ADVANCED_FACE('',(#895),#4560,.T.);
#4809=ADVANCED_FACE('',(#896,#478),#613,.F.);
#4810=ADVANCED_FACE('',(#897),#4561,.F.);
#4811=ADVANCED_FACE('',(#898),#4562,.T.);
#4812=ADVANCED_FACE('',(#899,#479),#614,.T.);
#4813=ADVANCED_FACE('',(#900,#480),#615,.F.);
#4814=ADVANCED_FACE('',(#901,#481),#616,.F.);
#4815=ADVANCED_FACE('',(#902,#482),#617,.T.);
#4816=ADVANCED_FACE('',(#903),#618,.T.);
#4817=ADVANCED_FACE('',(#904),#619,.T.);
#4818=ADVANCED_FACE('',(#905),#620,.T.);
#4819=ADVANCED_FACE('',(#906),#621,.T.);
#4820=ADVANCED_FACE('',(#907),#622,.T.);
#4821=ADVANCED_FACE('',(#908),#623,.T.);
#4822=ADVANCED_FACE('',(#909),#4563,.T.);
#4823=ADVANCED_FACE('',(#910,#483),#624,.T.);
#4824=ADVANCED_FACE('',(#911),#213,.T.);
#4825=ADVANCED_FACE('',(#912),#4564,.T.);
#4826=ADVANCED_FACE('',(#913),#214,.T.);
#4827=ADVANCED_FACE('',(#914,#484),#625,.T.);
#4828=ADVANCED_FACE('',(#915),#4565,.F.);
#4829=ADVANCED_FACE('',(#916),#626,.F.);
#4830=ADVANCED_FACE('',(#917),#627,.F.);
#4831=ADVANCED_FACE('',(#918),#628,.F.);
#4832=ADVANCED_FACE('',(#919),#629,.F.);
#4833=ADVANCED_FACE('',(#920),#630,.F.);
#4834=ADVANCED_FACE('',(#921),#631,.F.);
#4835=ADVANCED_FACE('',(#922),#632,.F.);
#4836=ADVANCED_FACE('',(#923,#485),#633,.T.);
#4837=ADVANCED_FACE('',(#924),#215,.T.);
#4838=ADVANCED_FACE('',(#925),#4566,.T.);
#4839=ADVANCED_FACE('',(#926),#216,.T.);
#4840=ADVANCED_FACE('',(#927),#634,.T.);
#4841=ADVANCED_FACE('',(#928),#635,.F.);
#4842=ADVANCED_FACE('',(#929),#636,.T.);
#4843=ADVANCED_FACE('',(#930),#637,.T.);
#4844=ADVANCED_FACE('',(#931),#638,.T.);
#4845=ADVANCED_FACE('',(#932),#639,.T.);
#4846=ADVANCED_FACE('',(#933),#640,.T.);
#4847=ADVANCED_FACE('',(#934),#641,.F.);
#4848=ADVANCED_FACE('',(#935),#642,.T.);
#4849=ADVANCED_FACE('',(#936),#643,.T.);
#4850=ADVANCED_FACE('',(#937),#644,.T.);
#4851=ADVANCED_FACE('',(#938),#645,.T.);
#4852=ADVANCED_FACE('',(#939),#217,.T.);
#4853=ADVANCED_FACE('',(#940),#4567,.T.);
#4854=ADVANCED_FACE('',(#941),#218,.T.);
#4855=ADVANCED_FACE('',(#942,#486),#646,.T.);
#4856=ADVANCED_FACE('',(#943),#219,.T.);
#4857=ADVANCED_FACE('',(#944),#4568,.T.);
#4858=ADVANCED_FACE('',(#945),#220,.T.);
#4859=ADVANCED_FACE('',(#946),#647,.T.);
#4860=ADVANCED_FACE('',(#947),#648,.F.);
#4861=ADVANCED_FACE('',(#948),#649,.F.);
#4862=ADVANCED_FACE('',(#949),#650,.F.);
#4863=ADVANCED_FACE('',(#950),#651,.F.);
#4864=ADVANCED_FACE('',(#951),#652,.F.);
#4865=ADVANCED_FACE('',(#952),#653,.F.);
#4866=ADVANCED_FACE('',(#953),#654,.F.);
#4867=ADVANCED_FACE('',(#954),#655,.F.);
#4868=CLOSED_SHELL('',(#4569,#4570,#4571,#4572,#4573,#4574,#4575,#4576,
#4577,#4578));
#4869=CLOSED_SHELL('',(#4579,#4580,#4581,#4582,#4583,#4584,#4585,#4586,
#4587,#4588,#4589,#4590,#4591,#4592,#4593,#4594,#4595,#4596,#4597,#4598,
#4599,#4600,#4601,#4602,#4603,#4604,#4605,#4606,#4607,#4608,#4609,#4610,
#4611,#4612,#4613,#4614,#4615,#4616,#4617,#4618,#4619,#4620,#4621));
#4870=CLOSED_SHELL('',(#4622,#4623,#4624,#4625,#4626,#4627,#4628,#4629));
#4871=CLOSED_SHELL('',(#4630));
#4872=CLOSED_SHELL('',(#4631,#4632,#4633,#4634,#4635,#4636,#4637,#4638));
#4873=CLOSED_SHELL('',(#4639));
#4874=CLOSED_SHELL('',(#4640,#4641,#4642,#4643,#4644,#4645,#4646,#4647));
#4875=CLOSED_SHELL('',(#4648,#4649,#4650,#4651,#4652,#4653,#4654,#4655,
#4656,#4657));
#4876=CLOSED_SHELL('',(#4658,#4659,#4660,#4661,#4662,#4663,#4664,#4665,
#4666,#4667));
#4877=CLOSED_SHELL('',(#4668,#4669,#4670,#4671,#4672,#4673));
#4878=CLOSED_SHELL('',(#4674,#4675,#4676,#4677,#4678,#4679));
#4879=CLOSED_SHELL('',(#4680,#4681,#4682,#4683,#4684,#4685,#4686,#4687));
#4880=CLOSED_SHELL('',(#4688,#4689,#4690,#4691,#4692,#4693,#4694,#4695));
#4881=CLOSED_SHELL('',(#4696));
#4882=CLOSED_SHELL('',(#4697));
#4883=CLOSED_SHELL('',(#4698));
#4884=CLOSED_SHELL('',(#4699));
#4885=CLOSED_SHELL('',(#4700));
#4886=CLOSED_SHELL('',(#4701));
#4887=CLOSED_SHELL('',(#4702));
#4888=CLOSED_SHELL('',(#4703));
#4889=CLOSED_SHELL('',(#4704,#4705,#4706,#4707,#4708,#4709,#4710,#4711,
#4712,#4713,#4714,#4715,#4716,#4717,#4718,#4719,#4720,#4721,#4722));
#4890=CLOSED_SHELL('',(#4723,#4724,#4725,#4726));
#4891=CLOSED_SHELL('',(#4727,#4728,#4729,#4730));
#4892=CLOSED_SHELL('',(#4731,#4732,#4733,#4734,#4735,#4736,#4737,#4738,
#4739));
#4893=CLOSED_SHELL('',(#4740,#4741,#4742,#4743,#4744,#4745,#4746,#4747));
#4894=CLOSED_SHELL('',(#4748,#4749,#4750,#4751,#4752,#4753,#4754,#4755,
#4756));
#4895=CLOSED_SHELL('',(#4757,#4758,#4759,#4760,#4761,#4762,#4763,#4764));
#4896=CLOSED_SHELL('',(#4765,#4766,#4767,#4768,#4769,#4770,#4771,#4772,
#4773,#4774,#4775,#4776,#4777,#4778,#4779,#4780,#4781,#4782,#4783,#4784,
#4785));
#4897=CLOSED_SHELL('',(#4786,#4787,#4788,#4789));
#4898=CLOSED_SHELL('',(#4790,#4791,#4792,#4793,#4794,#4795,#4796));
#4899=CLOSED_SHELL('',(#4797,#4798,#4799,#4800,#4801,#4802,#4803,#4804,
#4805,#4806,#4807,#4808,#4809));
#4900=CLOSED_SHELL('',(#4810,#4811,#4812,#4813));
#4901=CLOSED_SHELL('',(#4814,#4815,#4816,#4817,#4818,#4819,#4820,#4821,
#4822,#4823,#4824,#4825,#4826,#4827,#4828));
#4902=CLOSED_SHELL('',(#4829,#4830,#4831,#4832,#4833,#4834,#4835,#4836,
#4837,#4838,#4839,#4840));
#4903=CLOSED_SHELL('',(#4841,#4842,#4843,#4844,#4845,#4846,#4847,#4848,
#4849,#4850));
#4904=CLOSED_SHELL('',(#4851,#4852,#4853,#4854,#4855,#4856,#4857,#4858,
#4859));
#4905=CLOSED_SHELL('',(#4860,#4861,#4862,#4863,#4864,#4865,#4866,#4867));
#4906=DERIVED_UNIT_ELEMENT(#4960,1.);
#4907=DERIVED_UNIT_ELEMENT(#9450,-3.);
#4908=DERIVED_UNIT_ELEMENT(#4960,1.);
#4909=DERIVED_UNIT_ELEMENT(#9450,-3.);
#4910=DERIVED_UNIT_ELEMENT(#4960,1.);
#4911=DERIVED_UNIT_ELEMENT(#9450,-3.);
#4912=DERIVED_UNIT_ELEMENT(#4960,1.);
#4913=DERIVED_UNIT_ELEMENT(#9450,-3.);
#4914=DERIVED_UNIT_ELEMENT(#4960,1.);
#4915=DERIVED_UNIT_ELEMENT(#9450,-3.);
#4916=DERIVED_UNIT_ELEMENT(#4960,1.);
#4917=DERIVED_UNIT_ELEMENT(#9450,-3.);
#4918=DERIVED_UNIT_ELEMENT(#4960,1.);
#4919=DERIVED_UNIT_ELEMENT(#9450,-3.);
#4920=DERIVED_UNIT_ELEMENT(#4960,1.);
#4921=DERIVED_UNIT_ELEMENT(#9450,-3.);
#4922=DERIVED_UNIT_ELEMENT(#4960,1.);
#4923=DERIVED_UNIT_ELEMENT(#9450,-3.);
#4924=DERIVED_UNIT_ELEMENT(#4960,1.);
#4925=DERIVED_UNIT_ELEMENT(#9450,-3.);
#4926=DERIVED_UNIT_ELEMENT(#4960,1.);
#4927=DERIVED_UNIT_ELEMENT(#9450,-3.);
#4928=DERIVED_UNIT_ELEMENT(#4960,1.);
#4929=DERIVED_UNIT_ELEMENT(#9450,-3.);
#4930=DERIVED_UNIT_ELEMENT(#4960,1.);
#4931=DERIVED_UNIT_ELEMENT(#9450,-3.);
#4932=DERIVED_UNIT_ELEMENT(#4960,1.);
#4933=DERIVED_UNIT_ELEMENT(#9450,-3.);
#4934=DERIVED_UNIT_ELEMENT(#4960,1.);
#4935=DERIVED_UNIT_ELEMENT(#9450,-3.);
#4936=DERIVED_UNIT_ELEMENT(#4960,1.);
#4937=DERIVED_UNIT_ELEMENT(#9450,-3.);
#4938=DERIVED_UNIT_ELEMENT(#4960,1.);
#4939=DERIVED_UNIT_ELEMENT(#9450,-3.);
#4940=DERIVED_UNIT_ELEMENT(#4960,1.);
#4941=DERIVED_UNIT_ELEMENT(#9450,-3.);
#4942=DERIVED_UNIT_ELEMENT(#4960,1.);
#4943=DERIVED_UNIT_ELEMENT(#9450,-3.);
#4944=DERIVED_UNIT_ELEMENT(#4960,1.);
#4945=DERIVED_UNIT_ELEMENT(#9450,-3.);
#4946=DERIVED_UNIT_ELEMENT(#4960,1.);
#4947=DERIVED_UNIT_ELEMENT(#9450,-3.);
#4948=DERIVED_UNIT_ELEMENT(#4960,1.);
#4949=DERIVED_UNIT_ELEMENT(#9450,-3.);
#4950=DERIVED_UNIT_ELEMENT(#4960,1.);
#4951=DERIVED_UNIT_ELEMENT(#9450,-3.);
#4952=DERIVED_UNIT_ELEMENT(#4960,1.);
#4953=DERIVED_UNIT_ELEMENT(#9450,-3.);
#4954=DERIVED_UNIT_ELEMENT(#4960,1.);
#4955=DERIVED_UNIT_ELEMENT(#9450,-3.);
#4956=DERIVED_UNIT_ELEMENT(#4960,1.);
#4957=DERIVED_UNIT_ELEMENT(#9450,-3.);
#4958=DERIVED_UNIT_ELEMENT(#4960,1.);
#4959=DERIVED_UNIT_ELEMENT(#9450,-3.);
#4960=(
MASS_UNIT()
NAMED_UNIT(*)
SI_UNIT(.KILO.,.GRAM.)
);
#4961=DERIVED_UNIT((#4906,#4907));
#4962=DERIVED_UNIT((#4908,#4909));
#4963=DERIVED_UNIT((#4910,#4911));
#4964=DERIVED_UNIT((#4912,#4913));
#4965=DERIVED_UNIT((#4914,#4915));
#4966=DERIVED_UNIT((#4916,#4917));
#4967=DERIVED_UNIT((#4918,#4919));
#4968=DERIVED_UNIT((#4920,#4921));
#4969=DERIVED_UNIT((#4922,#4923));
#4970=DERIVED_UNIT((#4924,#4925));
#4971=DERIVED_UNIT((#4926,#4927));
#4972=DERIVED_UNIT((#4928,#4929));
#4973=DERIVED_UNIT((#4930,#4931));
#4974=DERIVED_UNIT((#4932,#4933));
#4975=DERIVED_UNIT((#4934,#4935));
#4976=DERIVED_UNIT((#4936,#4937));
#4977=DERIVED_UNIT((#4938,#4939));
#4978=DERIVED_UNIT((#4940,#4941));
#4979=DERIVED_UNIT((#4942,#4943));
#4980=DERIVED_UNIT((#4944,#4945));
#4981=DERIVED_UNIT((#4946,#4947));
#4982=DERIVED_UNIT((#4948,#4949));
#4983=DERIVED_UNIT((#4950,#4951));
#4984=DERIVED_UNIT((#4952,#4953));
#4985=DERIVED_UNIT((#4954,#4955));
#4986=DERIVED_UNIT((#4956,#4957));
#4987=DERIVED_UNIT((#4958,#4959));
#4988=MEASURE_REPRESENTATION_ITEM('density measure',
POSITIVE_RATIO_MEASURE(7850.),#4961);
#4989=MEASURE_REPRESENTATION_ITEM('density measure',
POSITIVE_RATIO_MEASURE(7850.),#4962);
#4990=MEASURE_REPRESENTATION_ITEM('density measure',
POSITIVE_RATIO_MEASURE(7850.),#4963);
#4991=MEASURE_REPRESENTATION_ITEM('density measure',
POSITIVE_RATIO_MEASURE(7850.),#4964);
#4992=MEASURE_REPRESENTATION_ITEM('density measure',
POSITIVE_RATIO_MEASURE(7850.),#4965);
#4993=MEASURE_REPRESENTATION_ITEM('density measure',
POSITIVE_RATIO_MEASURE(7850.),#4966);
#4994=MEASURE_REPRESENTATION_ITEM('density measure',
POSITIVE_RATIO_MEASURE(7850.),#4967);
#4995=MEASURE_REPRESENTATION_ITEM('density measure',
POSITIVE_RATIO_MEASURE(7850.),#4968);
#4996=MEASURE_REPRESENTATION_ITEM('density measure',
POSITIVE_RATIO_MEASURE(7850.),#4969);
#4997=MEASURE_REPRESENTATION_ITEM('density measure',
POSITIVE_RATIO_MEASURE(7850.),#4970);
#4998=MEASURE_REPRESENTATION_ITEM('density measure',
POSITIVE_RATIO_MEASURE(7850.),#4971);
#4999=MEASURE_REPRESENTATION_ITEM('density measure',
POSITIVE_RATIO_MEASURE(7850.),#4972);
#5000=MEASURE_REPRESENTATION_ITEM('density measure',
POSITIVE_RATIO_MEASURE(7850.),#4973);
#5001=MEASURE_REPRESENTATION_ITEM('density measure',
POSITIVE_RATIO_MEASURE(7850.),#4974);
#5002=MEASURE_REPRESENTATION_ITEM('density measure',
POSITIVE_RATIO_MEASURE(7850.),#4975);
#5003=MEASURE_REPRESENTATION_ITEM('density measure',
POSITIVE_RATIO_MEASURE(7850.),#4976);
#5004=MEASURE_REPRESENTATION_ITEM('density measure',
POSITIVE_RATIO_MEASURE(7850.),#4977);
#5005=MEASURE_REPRESENTATION_ITEM('density measure',
POSITIVE_RATIO_MEASURE(7850.),#4978);
#5006=MEASURE_REPRESENTATION_ITEM('density measure',
POSITIVE_RATIO_MEASURE(7850.),#4979);
#5007=MEASURE_REPRESENTATION_ITEM('density measure',
POSITIVE_RATIO_MEASURE(7850.),#4980);
#5008=MEASURE_REPRESENTATION_ITEM('density measure',
POSITIVE_RATIO_MEASURE(7850.),#4981);
#5009=MEASURE_REPRESENTATION_ITEM('density measure',
POSITIVE_RATIO_MEASURE(7850.),#4982);
#5010=MEASURE_REPRESENTATION_ITEM('density measure',
POSITIVE_RATIO_MEASURE(7850.),#4983);
#5011=MEASURE_REPRESENTATION_ITEM('density measure',
POSITIVE_RATIO_MEASURE(7850.),#4984);
#5012=MEASURE_REPRESENTATION_ITEM('density measure',
POSITIVE_RATIO_MEASURE(7850.),#4985);
#5013=MEASURE_REPRESENTATION_ITEM('density measure',
POSITIVE_RATIO_MEASURE(7850.),#4986);
#5014=MEASURE_REPRESENTATION_ITEM('density measure',
POSITIVE_RATIO_MEASURE(7850.),#4987);
#5015=PROPERTY_DEFINITION_REPRESENTATION(#5150,#5069);
#5016=PROPERTY_DEFINITION_REPRESENTATION(#5151,#5070);
#5017=PROPERTY_DEFINITION_REPRESENTATION(#5152,#5071);
#5018=PROPERTY_DEFINITION_REPRESENTATION(#5153,#5072);
#5019=PROPERTY_DEFINITION_REPRESENTATION(#5154,#5073);
#5020=PROPERTY_DEFINITION_REPRESENTATION(#5155,#5074);
#5021=PROPERTY_DEFINITION_REPRESENTATION(#5156,#5075);
#5022=PROPERTY_DEFINITION_REPRESENTATION(#5157,#5076);
#5023=PROPERTY_DEFINITION_REPRESENTATION(#5158,#5077);
#5024=PROPERTY_DEFINITION_REPRESENTATION(#5159,#5078);
#5025=PROPERTY_DEFINITION_REPRESENTATION(#5160,#5079);
#5026=PROPERTY_DEFINITION_REPRESENTATION(#5161,#5080);
#5027=PROPERTY_DEFINITION_REPRESENTATION(#5162,#5081);
#5028=PROPERTY_DEFINITION_REPRESENTATION(#5163,#5082);
#5029=PROPERTY_DEFINITION_REPRESENTATION(#5164,#5083);
#5030=PROPERTY_DEFINITION_REPRESENTATION(#5165,#5084);
#5031=PROPERTY_DEFINITION_REPRESENTATION(#5166,#5085);
#5032=PROPERTY_DEFINITION_REPRESENTATION(#5167,#5086);
#5033=PROPERTY_DEFINITION_REPRESENTATION(#5168,#5087);
#5034=PROPERTY_DEFINITION_REPRESENTATION(#5169,#5088);
#5035=PROPERTY_DEFINITION_REPRESENTATION(#5170,#5089);
#5036=PROPERTY_DEFINITION_REPRESENTATION(#5171,#5090);
#5037=PROPERTY_DEFINITION_REPRESENTATION(#5172,#5091);
#5038=PROPERTY_DEFINITION_REPRESENTATION(#5173,#5092);
#5039=PROPERTY_DEFINITION_REPRESENTATION(#5174,#5093);
#5040=PROPERTY_DEFINITION_REPRESENTATION(#5175,#5094);
#5041=PROPERTY_DEFINITION_REPRESENTATION(#5176,#5095);
#5042=PROPERTY_DEFINITION_REPRESENTATION(#5177,#5096);
#5043=PROPERTY_DEFINITION_REPRESENTATION(#5178,#5097);
#5044=PROPERTY_DEFINITION_REPRESENTATION(#5179,#5098);
#5045=PROPERTY_DEFINITION_REPRESENTATION(#5180,#5099);
#5046=PROPERTY_DEFINITION_REPRESENTATION(#5181,#5100);
#5047=PROPERTY_DEFINITION_REPRESENTATION(#5182,#5101);
#5048=PROPERTY_DEFINITION_REPRESENTATION(#5183,#5102);
#5049=PROPERTY_DEFINITION_REPRESENTATION(#5184,#5103);
#5050=PROPERTY_DEFINITION_REPRESENTATION(#5185,#5104);
#5051=PROPERTY_DEFINITION_REPRESENTATION(#5186,#5105);
#5052=PROPERTY_DEFINITION_REPRESENTATION(#5187,#5106);
#5053=PROPERTY_DEFINITION_REPRESENTATION(#5188,#5107);
#5054=PROPERTY_DEFINITION_REPRESENTATION(#5189,#5108);
#5055=PROPERTY_DEFINITION_REPRESENTATION(#5190,#5109);
#5056=PROPERTY_DEFINITION_REPRESENTATION(#5191,#5110);
#5057=PROPERTY_DEFINITION_REPRESENTATION(#5192,#5111);
#5058=PROPERTY_DEFINITION_REPRESENTATION(#5193,#5112);
#5059=PROPERTY_DEFINITION_REPRESENTATION(#5194,#5113);
#5060=PROPERTY_DEFINITION_REPRESENTATION(#5195,#5114);
#5061=PROPERTY_DEFINITION_REPRESENTATION(#5196,#5115);
#5062=PROPERTY_DEFINITION_REPRESENTATION(#5197,#5116);
#5063=PROPERTY_DEFINITION_REPRESENTATION(#5198,#5117);
#5064=PROPERTY_DEFINITION_REPRESENTATION(#5199,#5118);
#5065=PROPERTY_DEFINITION_REPRESENTATION(#5200,#5119);
#5066=PROPERTY_DEFINITION_REPRESENTATION(#5201,#5120);
#5067=PROPERTY_DEFINITION_REPRESENTATION(#5202,#5121);
#5068=PROPERTY_DEFINITION_REPRESENTATION(#5203,#5122);
#5069=REPRESENTATION('material name',(#5123),#9419);
#5070=REPRESENTATION('density',(#4988),#9419);
#5071=REPRESENTATION('material name',(#5124),#9420);
#5072=REPRESENTATION('density',(#4989),#9420);
#5073=REPRESENTATION('material name',(#5125),#9421);
#5074=REPRESENTATION('density',(#4990),#9421);
#5075=REPRESENTATION('material name',(#5126),#9422);
#5076=REPRESENTATION('density',(#4991),#9422);
#5077=REPRESENTATION('material name',(#5127),#9423);
#5078=REPRESENTATION('density',(#4992),#9423);
#5079=REPRESENTATION('material name',(#5128),#9424);
#5080=REPRESENTATION('density',(#4993),#9424);
#5081=REPRESENTATION('material name',(#5129),#9425);
#5082=REPRESENTATION('density',(#4994),#9425);
#5083=REPRESENTATION('material name',(#5130),#9426);
#5084=REPRESENTATION('density',(#4995),#9426);
#5085=REPRESENTATION('material name',(#5131),#9427);
#5086=REPRESENTATION('density',(#4996),#9427);
#5087=REPRESENTATION('material name',(#5132),#9428);
#5088=REPRESENTATION('density',(#4997),#9428);
#5089=REPRESENTATION('material name',(#5133),#9429);
#5090=REPRESENTATION('density',(#4998),#9429);
#5091=REPRESENTATION('material name',(#5134),#9431);
#5092=REPRESENTATION('density',(#4999),#9431);
#5093=REPRESENTATION('material name',(#5135),#9432);
#5094=REPRESENTATION('density',(#5000),#9432);
#5095=REPRESENTATION('material name',(#5136),#9433);
#5096=REPRESENTATION('density',(#5001),#9433);
#5097=REPRESENTATION('material name',(#5137),#9434);
#5098=REPRESENTATION('density',(#5002),#9434);
#5099=REPRESENTATION('material name',(#5138),#9435);
#5100=REPRESENTATION('density',(#5003),#9435);
#5101=REPRESENTATION('material name',(#5139),#9436);
#5102=REPRESENTATION('density',(#5004),#9436);
#5103=REPRESENTATION('material name',(#5140),#9437);
#5104=REPRESENTATION('density',(#5005),#9437);
#5105=REPRESENTATION('material name',(#5141),#9439);
#5106=REPRESENTATION('density',(#5006),#9439);
#5107=REPRESENTATION('material name',(#5142),#9440);
#5108=REPRESENTATION('density',(#5007),#9440);
#5109=REPRESENTATION('material name',(#5143),#9441);
#5110=REPRESENTATION('density',(#5008),#9441);
#5111=REPRESENTATION('material name',(#5144),#9442);
#5112=REPRESENTATION('density',(#5009),#9442);
#5113=REPRESENTATION('material name',(#5145),#9443);
#5114=REPRESENTATION('density',(#5010),#9443);
#5115=REPRESENTATION('material name',(#5146),#9444);
#5116=REPRESENTATION('density',(#5011),#9444);
#5117=REPRESENTATION('material name',(#5147),#9445);
#5118=REPRESENTATION('density',(#5012),#9445);
#5119=REPRESENTATION('material name',(#5148),#9446);
#5120=REPRESENTATION('density',(#5013),#9446);
#5121=REPRESENTATION('material name',(#5149),#9447);
#5122=REPRESENTATION('density',(#5014),#9447);
#5123=DESCRIPTIVE_REPRESENTATION_ITEM('Steel','Steel');
#5124=DESCRIPTIVE_REPRESENTATION_ITEM('Steel','Steel');
#5125=DESCRIPTIVE_REPRESENTATION_ITEM('Steel','Steel');
#5126=DESCRIPTIVE_REPRESENTATION_ITEM('Steel','Steel');
#5127=DESCRIPTIVE_REPRESENTATION_ITEM('Steel','Steel');
#5128=DESCRIPTIVE_REPRESENTATION_ITEM('Steel','Steel');
#5129=DESCRIPTIVE_REPRESENTATION_ITEM('Steel','Steel');
#5130=DESCRIPTIVE_REPRESENTATION_ITEM('Steel','Steel');
#5131=DESCRIPTIVE_REPRESENTATION_ITEM('Steel','Steel');
#5132=DESCRIPTIVE_REPRESENTATION_ITEM('Steel','Steel');
#5133=DESCRIPTIVE_REPRESENTATION_ITEM('Steel','Steel');
#5134=DESCRIPTIVE_REPRESENTATION_ITEM('Steel','Steel');
#5135=DESCRIPTIVE_REPRESENTATION_ITEM('Steel','Steel');
#5136=DESCRIPTIVE_REPRESENTATION_ITEM('Steel','Steel');
#5137=DESCRIPTIVE_REPRESENTATION_ITEM('Steel','Steel');
#5138=DESCRIPTIVE_REPRESENTATION_ITEM('Steel','Steel');
#5139=DESCRIPTIVE_REPRESENTATION_ITEM('Steel','Steel');
#5140=DESCRIPTIVE_REPRESENTATION_ITEM('Steel','Steel');
#5141=DESCRIPTIVE_REPRESENTATION_ITEM('Steel','Steel');
#5142=DESCRIPTIVE_REPRESENTATION_ITEM('Steel','Steel');
#5143=DESCRIPTIVE_REPRESENTATION_ITEM('Steel','Steel');
#5144=DESCRIPTIVE_REPRESENTATION_ITEM('Steel','Steel');
#5145=DESCRIPTIVE_REPRESENTATION_ITEM('Steel','Steel');
#5146=DESCRIPTIVE_REPRESENTATION_ITEM('Steel','Steel');
#5147=DESCRIPTIVE_REPRESENTATION_ITEM('Steel','Steel');
#5148=DESCRIPTIVE_REPRESENTATION_ITEM('Steel','Steel');
#5149=DESCRIPTIVE_REPRESENTATION_ITEM('Steel','Steel');
#5150=PROPERTY_DEFINITION('material property','material name',#9591);
#5151=PROPERTY_DEFINITION('material property','density of part',#9591);
#5152=PROPERTY_DEFINITION('material property','material name',#9592);
#5153=PROPERTY_DEFINITION('material property','density of part',#9592);
#5154=PROPERTY_DEFINITION('material property','material name',#9593);
#5155=PROPERTY_DEFINITION('material property','density of part',#9593);
#5156=PROPERTY_DEFINITION('material property','material name',#9594);
#5157=PROPERTY_DEFINITION('material property','density of part',#9594);
#5158=PROPERTY_DEFINITION('material property','material name',#9595);
#5159=PROPERTY_DEFINITION('material property','density of part',#9595);
#5160=PROPERTY_DEFINITION('material property','material name',#9596);
#5161=PROPERTY_DEFINITION('material property','density of part',#9596);
#5162=PROPERTY_DEFINITION('material property','material name',#9597);
#5163=PROPERTY_DEFINITION('material property','density of part',#9597);
#5164=PROPERTY_DEFINITION('material property','material name',#9598);
#5165=PROPERTY_DEFINITION('material property','density of part',#9598);
#5166=PROPERTY_DEFINITION('material property','material name',#9599);
#5167=PROPERTY_DEFINITION('material property','density of part',#9599);
#5168=PROPERTY_DEFINITION('material property','material name',#9600);
#5169=PROPERTY_DEFINITION('material property','density of part',#9600);
#5170=PROPERTY_DEFINITION('material property','material name',#9601);
#5171=PROPERTY_DEFINITION('material property','density of part',#9601);
#5172=PROPERTY_DEFINITION('material property','material name',#9603);
#5173=PROPERTY_DEFINITION('material property','density of part',#9603);
#5174=PROPERTY_DEFINITION('material property','material name',#9604);
#5175=PROPERTY_DEFINITION('material property','density of part',#9604);
#5176=PROPERTY_DEFINITION('material property','material name',#9605);
#5177=PROPERTY_DEFINITION('material property','density of part',#9605);
#5178=PROPERTY_DEFINITION('material property','material name',#9606);
#5179=PROPERTY_DEFINITION('material property','density of part',#9606);
#5180=PROPERTY_DEFINITION('material property','material name',#9607);
#5181=PROPERTY_DEFINITION('material property','density of part',#9607);
#5182=PROPERTY_DEFINITION('material property','material name',#9608);
#5183=PROPERTY_DEFINITION('material property','density of part',#9608);
#5184=PROPERTY_DEFINITION('material property','material name',#9609);
#5185=PROPERTY_DEFINITION('material property','density of part',#9609);
#5186=PROPERTY_DEFINITION('material property','material name',#9611);
#5187=PROPERTY_DEFINITION('material property','density of part',#9611);
#5188=PROPERTY_DEFINITION('material property','material name',#9612);
#5189=PROPERTY_DEFINITION('material property','density of part',#9612);
#5190=PROPERTY_DEFINITION('material property','material name',#9613);
#5191=PROPERTY_DEFINITION('material property','density of part',#9613);
#5192=PROPERTY_DEFINITION('material property','material name',#9614);
#5193=PROPERTY_DEFINITION('material property','density of part',#9614);
#5194=PROPERTY_DEFINITION('material property','material name',#9615);
#5195=PROPERTY_DEFINITION('material property','density of part',#9615);
#5196=PROPERTY_DEFINITION('material property','material name',#9616);
#5197=PROPERTY_DEFINITION('material property','density of part',#9616);
#5198=PROPERTY_DEFINITION('material property','material name',#9617);
#5199=PROPERTY_DEFINITION('material property','density of part',#9617);
#5200=PROPERTY_DEFINITION('material property','material name',#9618);
#5201=PROPERTY_DEFINITION('material property','density of part',#9618);
#5202=PROPERTY_DEFINITION('material property','material name',#9619);
#5203=PROPERTY_DEFINITION('material property','density of part',#9619);
#5204=AXIS2_PLACEMENT_3D('',#7396,#5828,#5829);
#5205=AXIS2_PLACEMENT_3D('',#7397,#5830,#5831);
#5206=AXIS2_PLACEMENT_3D('',#7398,#5832,#5833);
#5207=AXIS2_PLACEMENT_3D('',#7399,#5834,#5835);
#5208=AXIS2_PLACEMENT_3D('',#7401,#5836,#5837);
#5209=AXIS2_PLACEMENT_3D('',#7404,#5839,#5840);
#5210=AXIS2_PLACEMENT_3D('',#7405,#5841,#5842);
#5211=AXIS2_PLACEMENT_3D('',#7407,#5843,#5844);
#5212=AXIS2_PLACEMENT_3D('',#7410,#5846,#5847);
#5213=AXIS2_PLACEMENT_3D('',#7411,#5848,#5849);
#5214=AXIS2_PLACEMENT_3D('',#7413,#5850,#5851);
#5215=AXIS2_PLACEMENT_3D('',#7416,#5853,#5854);
#5216=AXIS2_PLACEMENT_3D('',#7417,#5855,#5856);
#5217=AXIS2_PLACEMENT_3D('',#7419,#5857,#5858);
#5218=AXIS2_PLACEMENT_3D('',#7422,#5860,#5861);
#5219=AXIS2_PLACEMENT_3D('',#7423,#5862,#5863);
#5220=AXIS2_PLACEMENT_3D('',#7432,#5868,#5869);
#5221=AXIS2_PLACEMENT_3D('',#7438,#5873,#5874);
#5222=AXIS2_PLACEMENT_3D('',#7444,#5878,#5879);
#5223=AXIS2_PLACEMENT_3D('',#7447,#5882,#5883);
#5224=AXIS2_PLACEMENT_3D('',#7448,#5884,#5885);
#5225=AXIS2_PLACEMENT_3D('',#7449,#5886,#5887);
#5226=AXIS2_PLACEMENT_3D('',#7450,#5888,#5889);
#5227=AXIS2_PLACEMENT_3D('',#7452,#5890,#5891);
#5228=AXIS2_PLACEMENT_3D('',#7455,#5893,#5894);
#5229=AXIS2_PLACEMENT_3D('',#7456,#5895,#5896);
#5230=AXIS2_PLACEMENT_3D('',#7457,#5897,#5898);
#5231=AXIS2_PLACEMENT_3D('',#7459,#5899,#5900);
#5232=AXIS2_PLACEMENT_3D('',#7462,#5902,#5903);
#5233=AXIS2_PLACEMENT_3D('',#7463,#5904,#5905);
#5234=AXIS2_PLACEMENT_3D('',#7464,#5906,#5907);
#5235=AXIS2_PLACEMENT_3D('',#7466,#5908,#5909);
#5236=AXIS2_PLACEMENT_3D('',#7469,#5911,#5912);
#5237=AXIS2_PLACEMENT_3D('',#7470,#5913,#5914);
#5238=AXIS2_PLACEMENT_3D('',#7471,#5915,#5916);
#5239=AXIS2_PLACEMENT_3D('',#7473,#5917,#5918);
#5240=AXIS2_PLACEMENT_3D('',#7476,#5920,#5921);
#5241=AXIS2_PLACEMENT_3D('',#7477,#5922,#5923);
#5242=AXIS2_PLACEMENT_3D('',#7478,#5924,#5925);
#5243=AXIS2_PLACEMENT_3D('',#7480,#5926,#5927);
#5244=AXIS2_PLACEMENT_3D('',#7483,#5929,#5930);
#5245=AXIS2_PLACEMENT_3D('',#7484,#5931,#5932);
#5246=AXIS2_PLACEMENT_3D('',#7485,#5933,#5934);
#5247=AXIS2_PLACEMENT_3D('',#7487,#5935,#5936);
#5248=AXIS2_PLACEMENT_3D('',#7490,#5938,#5939);
#5249=AXIS2_PLACEMENT_3D('',#7491,#5940,#5941);
#5250=AXIS2_PLACEMENT_3D('',#7492,#5942,#5943);
#5251=AXIS2_PLACEMENT_3D('',#7494,#5944,#5945);
#5252=AXIS2_PLACEMENT_3D('',#7497,#5947,#5948);
#5253=AXIS2_PLACEMENT_3D('',#7498,#5949,#5950);
#5254=AXIS2_PLACEMENT_3D('',#7499,#5951,#5952);
#5255=AXIS2_PLACEMENT_3D('',#7501,#5953,#5954);
#5256=AXIS2_PLACEMENT_3D('',#7504,#5956,#5957);
#5257=AXIS2_PLACEMENT_3D('',#7505,#5958,#5959);
#5258=AXIS2_PLACEMENT_3D('',#7506,#5960,#5961);
#5259=AXIS2_PLACEMENT_3D('',#7584,#5963,#5964);
#5260=AXIS2_PLACEMENT_3D('',#7586,#5965,#5966);
#5261=AXIS2_PLACEMENT_3D('',#7589,#5968,#5969);
#5262=AXIS2_PLACEMENT_3D('',#7590,#5970,#5971);
#5263=AXIS2_PLACEMENT_3D('',#7592,#5972,#5973);
#5264=AXIS2_PLACEMENT_3D('',#7595,#5975,#5976);
#5265=AXIS2_PLACEMENT_3D('',#7596,#5977,#5978);
#5266=AXIS2_PLACEMENT_3D('',#7598,#5979,#5980);
#5267=AXIS2_PLACEMENT_3D('',#7601,#5982,#5983);
#5268=AXIS2_PLACEMENT_3D('',#7602,#5984,#5985);
#5269=AXIS2_PLACEMENT_3D('',#7604,#5986,#5987);
#5270=AXIS2_PLACEMENT_3D('',#7607,#5989,#5990);
#5271=AXIS2_PLACEMENT_3D('',#7608,#5991,#5992);
#5272=AXIS2_PLACEMENT_3D('',#7611,#5993,#5994);
#5273=AXIS2_PLACEMENT_3D('',#7617,#5998,#5999);
#5274=AXIS2_PLACEMENT_3D('',#7619,#6000,#6001);
#5275=AXIS2_PLACEMENT_3D('',#7625,#6005,#6006);
#5276=AXIS2_PLACEMENT_3D('',#7628,#6007,#6008);
#5277=AXIS2_PLACEMENT_3D('',#7634,#6012,#6013);
#5278=AXIS2_PLACEMENT_3D('',#7636,#6014,#6015);
#5279=AXIS2_PLACEMENT_3D('',#7642,#6019,#6020);
#5280=AXIS2_PLACEMENT_3D('',#7645,#6023,#6024);
#5281=AXIS2_PLACEMENT_3D('',#7648,#6027,#6028);
#5282=AXIS2_PLACEMENT_3D('',#7650,#6030,#6031);
#5283=AXIS2_PLACEMENT_3D('',#7652,#6033,#6034);
#5284=AXIS2_PLACEMENT_3D('',#7653,#6035,#6036);
#5285=AXIS2_PLACEMENT_3D('',#7656,#6037,#6038);
#5286=AXIS2_PLACEMENT_3D('',#7662,#6042,#6043);
#5287=AXIS2_PLACEMENT_3D('',#7664,#6044,#6045);
#5288=AXIS2_PLACEMENT_3D('',#7670,#6049,#6050);
#5289=AXIS2_PLACEMENT_3D('',#7673,#6051,#6052);
#5290=AXIS2_PLACEMENT_3D('',#7679,#6056,#6057);
#5291=AXIS2_PLACEMENT_3D('',#7681,#6058,#6059);
#5292=AXIS2_PLACEMENT_3D('',#7687,#6063,#6064);
#5293=AXIS2_PLACEMENT_3D('',#7690,#6067,#6068);
#5294=AXIS2_PLACEMENT_3D('',#7693,#6071,#6072);
#5295=AXIS2_PLACEMENT_3D('',#7695,#6074,#6075);
#5296=AXIS2_PLACEMENT_3D('',#7697,#6077,#6078);
#5297=AXIS2_PLACEMENT_3D('',#7698,#6079,#6080);
#5298=AXIS2_PLACEMENT_3D('',#7700,#6081,#6082);
#5299=AXIS2_PLACEMENT_3D('',#7703,#6084,#6085);
#5300=AXIS2_PLACEMENT_3D('',#7704,#6086,#6087);
#5301=AXIS2_PLACEMENT_3D('',#7706,#6088,#6089);
#5302=AXIS2_PLACEMENT_3D('',#7709,#6091,#6092);
#5303=AXIS2_PLACEMENT_3D('',#7710,#6093,#6094);
#5304=AXIS2_PLACEMENT_3D('',#7711,#6095,#6096);
#5305=AXIS2_PLACEMENT_3D('',#7712,#6097,#6098);
#5306=AXIS2_PLACEMENT_3D('',#7713,#6099,#6100);
#5307=AXIS2_PLACEMENT_3D('',#7715,#6101,#6102);
#5308=AXIS2_PLACEMENT_3D('',#7718,#6104,#6105);
#5309=AXIS2_PLACEMENT_3D('',#7719,#6106,#6107);
#5310=AXIS2_PLACEMENT_3D('',#7721,#6108,#6109);
#5311=AXIS2_PLACEMENT_3D('',#7722,#6110,#6111);
#5312=AXIS2_PLACEMENT_3D('',#7724,#6112,#6113);
#5313=AXIS2_PLACEMENT_3D('',#7725,#6114,#6115);
#5314=AXIS2_PLACEMENT_3D('',#7728,#6117,#6118);
#5315=AXIS2_PLACEMENT_3D('',#7729,#6119,#6120);
#5316=AXIS2_PLACEMENT_3D('',#7731,#6121,#6122);
#5317=AXIS2_PLACEMENT_3D('',#7733,#6124,#6125);
#5318=AXIS2_PLACEMENT_3D('',#7735,#6126,#6127);
#5319=AXIS2_PLACEMENT_3D('',#7738,#6129,#6130);
#5320=AXIS2_PLACEMENT_3D('',#7739,#6131,#6132);
#5321=AXIS2_PLACEMENT_3D('',#7740,#6133,#6134);
#5322=AXIS2_PLACEMENT_3D('',#7741,#6135,#6136);
#5323=AXIS2_PLACEMENT_3D('',#7742,#6137,#6138);
#5324=AXIS2_PLACEMENT_3D('',#7744,#6139,#6140);
#5325=AXIS2_PLACEMENT_3D('',#7745,#6141,#6142);
#5326=AXIS2_PLACEMENT_3D('',#7746,#6143,#6144);
#5327=AXIS2_PLACEMENT_3D('',#7747,#6145,#6146);
#5328=AXIS2_PLACEMENT_3D('',#7749,#6147,#6148);
#5329=AXIS2_PLACEMENT_3D('',#7752,#6150,#6151);
#5330=AXIS2_PLACEMENT_3D('',#7753,#6152,#6153);
#5331=AXIS2_PLACEMENT_3D('',#7755,#6154,#6155);
#5332=AXIS2_PLACEMENT_3D('',#7756,#6156,#6157);
#5333=AXIS2_PLACEMENT_3D('',#7758,#6158,#6159);
#5334=AXIS2_PLACEMENT_3D('',#7759,#6160,#6161);
#5335=AXIS2_PLACEMENT_3D('',#7762,#6163,#6164);
#5336=AXIS2_PLACEMENT_3D('',#7763,#6165,#6166);
#5337=AXIS2_PLACEMENT_3D('',#7765,#6167,#6168);
#5338=AXIS2_PLACEMENT_3D('',#7767,#6170,#6171);
#5339=AXIS2_PLACEMENT_3D('',#7769,#6172,#6173);
#5340=AXIS2_PLACEMENT_3D('',#7772,#6175,#6176);
#5341=AXIS2_PLACEMENT_3D('',#7773,#6177,#6178);
#5342=AXIS2_PLACEMENT_3D('',#7774,#6179,#6180);
#5343=AXIS2_PLACEMENT_3D('',#7775,#6181,#6182);
#5344=AXIS2_PLACEMENT_3D('',#7776,#6183,#6184);
#5345=AXIS2_PLACEMENT_3D('',#7778,#6185,#6186);
#5346=AXIS2_PLACEMENT_3D('',#7779,#6187,#6188);
#5347=AXIS2_PLACEMENT_3D('',#7780,#6189,#6190);
#5348=AXIS2_PLACEMENT_3D('',#7781,#6191,#6192);
#5349=AXIS2_PLACEMENT_3D('',#7803,#6195,#6196);
#5350=AXIS2_PLACEMENT_3D('',#7804,#6197,#6198);
#5351=AXIS2_PLACEMENT_3D('',#7809,#6200,#6201);
#5352=AXIS2_PLACEMENT_3D('',#7826,#6203,#6204);
#5353=AXIS2_PLACEMENT_3D('',#7830,#6207,#6208);
#5354=AXIS2_PLACEMENT_3D('',#7831,#6209,#6210);
#5355=AXIS2_PLACEMENT_3D('',#7832,#6211,#6212);
#5356=AXIS2_PLACEMENT_3D('',#7834,#6213,#6214);
#5357=AXIS2_PLACEMENT_3D('',#7835,#6215,#6216);
#5358=AXIS2_PLACEMENT_3D('',#7836,#6217,#6218);
#5359=AXIS2_PLACEMENT_3D('',#7837,#6219,#6220);
#5360=AXIS2_PLACEMENT_3D('',#7877,#6222,#6223);
#5361=AXIS2_PLACEMENT_3D('',#7880,#6225,#6226);
#5362=AXIS2_PLACEMENT_3D('',#7881,#6227,#6228);
#5363=AXIS2_PLACEMENT_3D('',#7882,#6229,#6230);
#5364=AXIS2_PLACEMENT_3D('',#7883,#6231,#6232);
#5365=AXIS2_PLACEMENT_3D('',#7885,#6233,#6234);
#5366=AXIS2_PLACEMENT_3D('',#7888,#6236,#6237);
#5367=AXIS2_PLACEMENT_3D('',#7889,#6238,#6239);
#5368=AXIS2_PLACEMENT_3D('',#7891,#6240,#6241);
#5369=AXIS2_PLACEMENT_3D('',#7894,#6243,#6244);
#5370=AXIS2_PLACEMENT_3D('',#7895,#6245,#6246);
#5371=AXIS2_PLACEMENT_3D('',#7897,#6247,#6248);
#5372=AXIS2_PLACEMENT_3D('',#7900,#6250,#6251);
#5373=AXIS2_PLACEMENT_3D('',#7901,#6252,#6253);
#5374=AXIS2_PLACEMENT_3D('',#7903,#6254,#6255);
#5375=AXIS2_PLACEMENT_3D('',#7906,#6257,#6258);
#5376=AXIS2_PLACEMENT_3D('',#7907,#6259,#6260);
#5377=AXIS2_PLACEMENT_3D('',#7909,#6261,#6262);
#5378=AXIS2_PLACEMENT_3D('',#7912,#6264,#6265);
#5379=AXIS2_PLACEMENT_3D('',#7913,#6266,#6267);
#5380=AXIS2_PLACEMENT_3D('',#7915,#6268,#6269);
#5381=AXIS2_PLACEMENT_3D('',#7916,#6270,#6271);
#5382=AXIS2_PLACEMENT_3D('',#7919,#6273,#6274);
#5383=AXIS2_PLACEMENT_3D('',#7920,#6275,#6276);
#5384=AXIS2_PLACEMENT_3D('',#7922,#6277,#6278);
#5385=AXIS2_PLACEMENT_3D('',#7925,#6280,#6281);
#5386=AXIS2_PLACEMENT_3D('',#7926,#6282,#6283);
#5387=AXIS2_PLACEMENT_3D('',#7927,#6284,#6285);
#5388=AXIS2_PLACEMENT_3D('',#7928,#6286,#6287);
#5389=AXIS2_PLACEMENT_3D('',#7929,#6288,#6289);
#5390=AXIS2_PLACEMENT_3D('',#7931,#6290,#6291);
#5391=AXIS2_PLACEMENT_3D('',#7934,#6293,#6294);
#5392=AXIS2_PLACEMENT_3D('',#7935,#6295,#6296);
#5393=AXIS2_PLACEMENT_3D('',#7937,#6297,#6298);
#5394=AXIS2_PLACEMENT_3D('',#7940,#6300,#6301);
#5395=AXIS2_PLACEMENT_3D('',#7941,#6302,#6303);
#5396=AXIS2_PLACEMENT_3D('',#7943,#6304,#6305);
#5397=AXIS2_PLACEMENT_3D('',#7946,#6307,#6308);
#5398=AXIS2_PLACEMENT_3D('',#7947,#6309,#6310);
#5399=AXIS2_PLACEMENT_3D('',#7949,#6311,#6312);
#5400=AXIS2_PLACEMENT_3D('',#7952,#6314,#6315);
#5401=AXIS2_PLACEMENT_3D('',#7953,#6316,#6317);
#5402=AXIS2_PLACEMENT_3D('',#7955,#6318,#6319);
#5403=AXIS2_PLACEMENT_3D('',#7958,#6321,#6322);
#5404=AXIS2_PLACEMENT_3D('',#7959,#6323,#6324);
#5405=AXIS2_PLACEMENT_3D('',#7961,#6325,#6326);
#5406=AXIS2_PLACEMENT_3D('',#7962,#6327,#6328);
#5407=AXIS2_PLACEMENT_3D('',#7964,#6329,#6330);
#5408=AXIS2_PLACEMENT_3D('',#7966,#6332,#6333);
#5409=AXIS2_PLACEMENT_3D('',#7968,#6334,#6335);
#5410=AXIS2_PLACEMENT_3D('',#7971,#6337,#6338);
#5411=AXIS2_PLACEMENT_3D('',#7972,#6339,#6340);
#5412=AXIS2_PLACEMENT_3D('',#7973,#6341,#6342);
#5413=AXIS2_PLACEMENT_3D('',#7974,#6343,#6344);
#5414=AXIS2_PLACEMENT_3D('',#7975,#6345,#6346);
#5415=AXIS2_PLACEMENT_3D('',#7984,#6351,#6352);
#5416=AXIS2_PLACEMENT_3D('',#7990,#6356,#6357);
#5417=AXIS2_PLACEMENT_3D('',#7996,#6361,#6362);
#5418=AXIS2_PLACEMENT_3D('',#7999,#6365,#6366);
#5419=AXIS2_PLACEMENT_3D('',#8000,#6367,#6368);
#5420=AXIS2_PLACEMENT_3D('',#8001,#6369,#6370);
#5421=AXIS2_PLACEMENT_3D('',#8002,#6371,#6372);
#5422=AXIS2_PLACEMENT_3D('',#8011,#6377,#6378);
#5423=AXIS2_PLACEMENT_3D('',#8017,#6382,#6383);
#5424=AXIS2_PLACEMENT_3D('',#8023,#6387,#6388);
#5425=AXIS2_PLACEMENT_3D('',#8026,#6391,#6392);
#5426=AXIS2_PLACEMENT_3D('',#8027,#6393,#6394);
#5427=AXIS2_PLACEMENT_3D('',#8028,#6395,#6396);
#5428=AXIS2_PLACEMENT_3D('',#8029,#6397,#6398);
#5429=AXIS2_PLACEMENT_3D('',#8030,#6399,#6400);
#5430=AXIS2_PLACEMENT_3D('',#8033,#6401,#6402);
#5431=AXIS2_PLACEMENT_3D('',#8034,#6403,#6404);
#5432=AXIS2_PLACEMENT_3D('',#8036,#6405,#6406);
#5433=AXIS2_PLACEMENT_3D('',#8038,#6407,#6408);
#5434=AXIS2_PLACEMENT_3D('',#8039,#6409,#6410);
#5435=AXIS2_PLACEMENT_3D('',#8040,#6411,#6412);
#5436=AXIS2_PLACEMENT_3D('',#8043,#6414,#6415);
#5437=AXIS2_PLACEMENT_3D('',#8044,#6416,#6417);
#5438=AXIS2_PLACEMENT_3D('',#8046,#6418,#6419);
#5439=AXIS2_PLACEMENT_3D('',#8049,#6421,#6422);
#5440=AXIS2_PLACEMENT_3D('',#8050,#6423,#6424);
#5441=AXIS2_PLACEMENT_3D('',#8053,#6426,#6427);
#5442=AXIS2_PLACEMENT_3D('',#8054,#6428,#6429);
#5443=AXIS2_PLACEMENT_3D('',#8055,#6430,#6431);
#5444=AXIS2_PLACEMENT_3D('',#8057,#6432,#6433);
#5445=AXIS2_PLACEMENT_3D('',#8059,#6435,#6436);
#5446=AXIS2_PLACEMENT_3D('',#8061,#6437,#6438);
#5447=AXIS2_PLACEMENT_3D('',#8062,#6439,#6440);
#5448=AXIS2_PLACEMENT_3D('',#8064,#6442,#6443);
#5449=AXIS2_PLACEMENT_3D('',#8065,#6444,#6445);
#5450=AXIS2_PLACEMENT_3D('',#8068,#6446,#6447);
#5451=AXIS2_PLACEMENT_3D('',#8069,#6448,#6449);
#5452=AXIS2_PLACEMENT_3D('',#8071,#6450,#6451);
#5453=AXIS2_PLACEMENT_3D('',#8073,#6452,#6453);
#5454=AXIS2_PLACEMENT_3D('',#8074,#6454,#6455);
#5455=AXIS2_PLACEMENT_3D('',#8075,#6456,#6457);
#5456=AXIS2_PLACEMENT_3D('',#8077,#6458,#6459);
#5457=AXIS2_PLACEMENT_3D('',#8079,#6461,#6462);
#5458=AXIS2_PLACEMENT_3D('',#8081,#6463,#6464);
#5459=AXIS2_PLACEMENT_3D('',#8083,#6465,#6466);
#5460=AXIS2_PLACEMENT_3D('',#8084,#6467,#6468);
#5461=AXIS2_PLACEMENT_3D('',#8086,#6469,#6470);
#5462=AXIS2_PLACEMENT_3D('',#8088,#6472,#6473);
#5463=AXIS2_PLACEMENT_3D('',#8090,#6474,#6475);
#5464=AXIS2_PLACEMENT_3D('',#8092,#6477,#6478);
#5465=AXIS2_PLACEMENT_3D('',#8094,#6479,#6480);
#5466=AXIS2_PLACEMENT_3D('',#8096,#6482,#6483);
#5467=AXIS2_PLACEMENT_3D('',#8097,#6484,#6485);
#5468=AXIS2_PLACEMENT_3D('',#8099,#6487,#6488);
#5469=AXIS2_PLACEMENT_3D('',#8100,#6489,#6490);
#5470=AXIS2_PLACEMENT_3D('',#8103,#6491,#6492);
#5471=AXIS2_PLACEMENT_3D('',#8104,#6493,#6494);
#5472=AXIS2_PLACEMENT_3D('',#8107,#6495,#6496);
#5473=AXIS2_PLACEMENT_3D('',#8108,#6497,#6498);
#5474=AXIS2_PLACEMENT_3D('',#8111,#6499,#6500);
#5475=AXIS2_PLACEMENT_3D('',#8112,#6501,#6502);
#5476=AXIS2_PLACEMENT_3D('',#8115,#6503,#6504);
#5477=AXIS2_PLACEMENT_3D('',#8116,#6505,#6506);
#5478=AXIS2_PLACEMENT_3D('',#8119,#6507,#6508);
#5479=AXIS2_PLACEMENT_3D('',#8120,#6509,#6510);
#5480=AXIS2_PLACEMENT_3D('',#8123,#6511,#6512);
#5481=AXIS2_PLACEMENT_3D('',#8124,#6513,#6514);
#5482=AXIS2_PLACEMENT_3D('',#8127,#6515,#6516);
#5483=AXIS2_PLACEMENT_3D('',#8128,#6517,#6518);
#5484=AXIS2_PLACEMENT_3D('',#8131,#6519,#6520);
#5485=AXIS2_PLACEMENT_3D('',#8132,#6521,#6522);
#5486=AXIS2_PLACEMENT_3D('',#8133,#6523,#6524);
#5487=AXIS2_PLACEMENT_3D('',#8159,#6525,#6526);
#5488=AXIS2_PLACEMENT_3D('',#8183,#6527,#6528);
#5489=AXIS2_PLACEMENT_3D('',#8184,#6529,#6530);
#5490=AXIS2_PLACEMENT_3D('',#8186,#6531,#6532);
#5491=AXIS2_PLACEMENT_3D('',#8211,#6533,#6534);
#5492=AXIS2_PLACEMENT_3D('',#8236,#6535,#6536);
#5493=AXIS2_PLACEMENT_3D('',#8252,#6538,#6539);
#5494=AXIS2_PLACEMENT_3D('',#8267,#6540,#6541);
#5495=AXIS2_PLACEMENT_3D('',#8292,#6542,#6543);
#5496=AXIS2_PLACEMENT_3D('',#8317,#6544,#6545);
#5497=AXIS2_PLACEMENT_3D('',#8342,#6546,#6547);
#5498=AXIS2_PLACEMENT_3D('',#8366,#6548,#6549);
#5499=AXIS2_PLACEMENT_3D('',#8367,#6550,#6551);
#5500=AXIS2_PLACEMENT_3D('',#8369,#6552,#6553);
#5501=AXIS2_PLACEMENT_3D('',#8370,#6554,#6555);
#5502=AXIS2_PLACEMENT_3D('',#8371,#6556,#6557);
#5503=AXIS2_PLACEMENT_3D('',#8395,#6558,#6559);
#5504=AXIS2_PLACEMENT_3D('',#8396,#6560,#6561);
#5505=AXIS2_PLACEMENT_3D('',#8398,#6562,#6563);
#5506=AXIS2_PLACEMENT_3D('',#8399,#6564,#6565);
#5507=AXIS2_PLACEMENT_3D('',#8400,#6566,#6567);
#5508=AXIS2_PLACEMENT_3D('',#8424,#6568,#6569);
#5509=AXIS2_PLACEMENT_3D('',#8425,#6570,#6571);
#5510=AXIS2_PLACEMENT_3D('',#8427,#6572,#6573);
#5511=AXIS2_PLACEMENT_3D('',#8428,#6574,#6575);
#5512=AXIS2_PLACEMENT_3D('',#8429,#6576,#6577);
#5513=AXIS2_PLACEMENT_3D('',#8444,#6578,#6579);
#5514=AXIS2_PLACEMENT_3D('',#8457,#6580,#6581);
#5515=AXIS2_PLACEMENT_3D('',#8459,#6582,#6583);
#5516=AXIS2_PLACEMENT_3D('',#8460,#6584,#6585);
#5517=AXIS2_PLACEMENT_3D('',#8461,#6586,#6587);
#5518=AXIS2_PLACEMENT_3D('',#8485,#6588,#6589);
#5519=AXIS2_PLACEMENT_3D('',#8486,#6590,#6591);
#5520=AXIS2_PLACEMENT_3D('',#8488,#6592,#6593);
#5521=AXIS2_PLACEMENT_3D('',#8489,#6594,#6595);
#5522=AXIS2_PLACEMENT_3D('',#8490,#6596,#6597);
#5523=AXIS2_PLACEMENT_3D('',#8514,#6598,#6599);
#5524=AXIS2_PLACEMENT_3D('',#8515,#6600,#6601);
#5525=AXIS2_PLACEMENT_3D('',#8517,#6602,#6603);
#5526=AXIS2_PLACEMENT_3D('',#8518,#6604,#6605);
#5527=AXIS2_PLACEMENT_3D('',#8519,#6606,#6607);
#5528=AXIS2_PLACEMENT_3D('',#8543,#6608,#6609);
#5529=AXIS2_PLACEMENT_3D('',#8544,#6610,#6611);
#5530=AXIS2_PLACEMENT_3D('',#8546,#6612,#6613);
#5531=AXIS2_PLACEMENT_3D('',#8549,#6615,#6616);
#5532=AXIS2_PLACEMENT_3D('',#8573,#6617,#6618);
#5533=AXIS2_PLACEMENT_3D('',#8574,#6619,#6620);
#5534=AXIS2_PLACEMENT_3D('',#8575,#6621,#6622);
#5535=AXIS2_PLACEMENT_3D('',#8576,#6623,#6624);
#5536=AXIS2_PLACEMENT_3D('',#8577,#6625,#6626);
#5537=AXIS2_PLACEMENT_3D('',#8578,#6627,#6628);
#5538=AXIS2_PLACEMENT_3D('',#8579,#6629,#6630);
#5539=AXIS2_PLACEMENT_3D('',#8580,#6631,#6632);
#5540=AXIS2_PLACEMENT_3D('',#8581,#6633,#6634);
#5541=AXIS2_PLACEMENT_3D('',#8583,#6635,#6636);
#5542=AXIS2_PLACEMENT_3D('',#8585,#6637,#6638);
#5543=AXIS2_PLACEMENT_3D('',#8586,#6639,#6640);
#5544=AXIS2_PLACEMENT_3D('',#8588,#6641,#6642);
#5545=AXIS2_PLACEMENT_3D('',#8590,#6644,#6645);
#5546=AXIS2_PLACEMENT_3D('',#8592,#6646,#6647);
#5547=AXIS2_PLACEMENT_3D('',#8593,#6648,#6649);
#5548=AXIS2_PLACEMENT_3D('',#8595,#6651,#6652);
#5549=AXIS2_PLACEMENT_3D('',#8597,#6653,#6654);
#5550=AXIS2_PLACEMENT_3D('',#8599,#6655,#6656);
#5551=AXIS2_PLACEMENT_3D('',#8600,#6657,#6658);
#5552=AXIS2_PLACEMENT_3D('',#8602,#6659,#6660);
#5553=AXIS2_PLACEMENT_3D('',#8604,#6662,#6663);
#5554=AXIS2_PLACEMENT_3D('',#8606,#6664,#6665);
#5555=AXIS2_PLACEMENT_3D('',#8607,#6666,#6667);
#5556=AXIS2_PLACEMENT_3D('',#8609,#6669,#6670);
#5557=AXIS2_PLACEMENT_3D('',#8610,#6671,#6672);
#5558=AXIS2_PLACEMENT_3D('',#8611,#6673,#6674);
#5559=AXIS2_PLACEMENT_3D('',#8612,#6675,#6676);
#5560=AXIS2_PLACEMENT_3D('',#8613,#6677,#6678);
#5561=AXIS2_PLACEMENT_3D('',#8614,#6679,#6680);
#5562=AXIS2_PLACEMENT_3D('',#8615,#6681,#6682);
#5563=AXIS2_PLACEMENT_3D('',#8617,#6683,#6684);
#5564=AXIS2_PLACEMENT_3D('',#8618,#6685,#6686);
#5565=AXIS2_PLACEMENT_3D('',#8620,#6687,#6688);
#5566=AXIS2_PLACEMENT_3D('',#8622,#6690,#6691);
#5567=AXIS2_PLACEMENT_3D('',#8624,#6692,#6693);
#5568=AXIS2_PLACEMENT_3D('',#8626,#6695,#6696);
#5569=AXIS2_PLACEMENT_3D('',#8628,#6697,#6698);
#5570=AXIS2_PLACEMENT_3D('',#8630,#6700,#6701);
#5571=AXIS2_PLACEMENT_3D('',#8632,#6702,#6703);
#5572=AXIS2_PLACEMENT_3D('',#8633,#6704,#6705);
#5573=AXIS2_PLACEMENT_3D('',#8635,#6706,#6707);
#5574=AXIS2_PLACEMENT_3D('',#8637,#6709,#6710);
#5575=AXIS2_PLACEMENT_3D('',#8639,#6711,#6712);
#5576=AXIS2_PLACEMENT_3D('',#8641,#6714,#6715);
#5577=AXIS2_PLACEMENT_3D('',#8643,#6716,#6717);
#5578=AXIS2_PLACEMENT_3D('',#8645,#6719,#6720);
#5579=AXIS2_PLACEMENT_3D('',#8646,#6721,#6722);
#5580=AXIS2_PLACEMENT_3D('',#8655,#6727,#6728);
#5581=AXIS2_PLACEMENT_3D('',#8661,#6732,#6733);
#5582=AXIS2_PLACEMENT_3D('',#8667,#6737,#6738);
#5583=AXIS2_PLACEMENT_3D('',#8673,#6742,#6743);
#5584=AXIS2_PLACEMENT_3D('',#8679,#6747,#6748);
#5585=AXIS2_PLACEMENT_3D('',#8682,#6751,#6752);
#5586=AXIS2_PLACEMENT_3D('',#8683,#6753,#6754);
#5587=AXIS2_PLACEMENT_3D('',#8684,#6755,#6756);
#5588=AXIS2_PLACEMENT_3D('',#8685,#6757,#6758);
#5589=AXIS2_PLACEMENT_3D('',#8687,#6759,#6760);
#5590=AXIS2_PLACEMENT_3D('',#8688,#6761,#6762);
#5591=AXIS2_PLACEMENT_3D('',#8690,#6763,#6764);
#5592=AXIS2_PLACEMENT_3D('',#8692,#6766,#6767);
#5593=AXIS2_PLACEMENT_3D('',#8694,#6768,#6769);
#5594=AXIS2_PLACEMENT_3D('',#8696,#6771,#6772);
#5595=AXIS2_PLACEMENT_3D('',#8698,#6773,#6774);
#5596=AXIS2_PLACEMENT_3D('',#8700,#6776,#6777);
#5597=AXIS2_PLACEMENT_3D('',#8702,#6778,#6779);
#5598=AXIS2_PLACEMENT_3D('',#8703,#6780,#6781);
#5599=AXIS2_PLACEMENT_3D('',#8705,#6782,#6783);
#5600=AXIS2_PLACEMENT_3D('',#8707,#6785,#6786);
#5601=AXIS2_PLACEMENT_3D('',#8709,#6787,#6788);
#5602=AXIS2_PLACEMENT_3D('',#8711,#6790,#6791);
#5603=AXIS2_PLACEMENT_3D('',#8713,#6792,#6793);
#5604=AXIS2_PLACEMENT_3D('',#8715,#6795,#6796);
#5605=AXIS2_PLACEMENT_3D('',#8716,#6797,#6798);
#5606=AXIS2_PLACEMENT_3D('',#8725,#6803,#6804);
#5607=AXIS2_PLACEMENT_3D('',#8731,#6808,#6809);
#5608=AXIS2_PLACEMENT_3D('',#8737,#6813,#6814);
#5609=AXIS2_PLACEMENT_3D('',#8743,#6818,#6819);
#5610=AXIS2_PLACEMENT_3D('',#8749,#6823,#6824);
#5611=AXIS2_PLACEMENT_3D('',#8752,#6827,#6828);
#5612=AXIS2_PLACEMENT_3D('',#8753,#6829,#6830);
#5613=AXIS2_PLACEMENT_3D('',#8754,#6831,#6832);
#5614=AXIS2_PLACEMENT_3D('',#8755,#6833,#6834);
#5615=AXIS2_PLACEMENT_3D('',#8756,#6835,#6836);
#5616=AXIS2_PLACEMENT_3D('',#8758,#6837,#6838);
#5617=AXIS2_PLACEMENT_3D('',#8761,#6840,#6841);
#5618=AXIS2_PLACEMENT_3D('',#8762,#6842,#6843);
#5619=AXIS2_PLACEMENT_3D('',#8763,#6844,#6845);
#5620=AXIS2_PLACEMENT_3D('',#8772,#6850,#6851);
#5621=AXIS2_PLACEMENT_3D('',#8774,#6852,#6853);
#5622=AXIS2_PLACEMENT_3D('',#8778,#6856,#6857);
#5623=AXIS2_PLACEMENT_3D('',#8784,#6861,#6862);
#5624=AXIS2_PLACEMENT_3D('',#8786,#6864,#6865);
#5625=AXIS2_PLACEMENT_3D('',#8788,#6866,#6867);
#5626=AXIS2_PLACEMENT_3D('',#8791,#6869,#6870);
#5627=AXIS2_PLACEMENT_3D('',#8792,#6871,#6872);
#5628=AXIS2_PLACEMENT_3D('',#8831,#6873,#6874);
#5629=AXIS2_PLACEMENT_3D('',#8833,#6875,#6876);
#5630=AXIS2_PLACEMENT_3D('',#8834,#6877,#6878);
#5631=AXIS2_PLACEMENT_3D('',#8836,#6879,#6880);
#5632=AXIS2_PLACEMENT_3D('',#8837,#6881,#6882);
#5633=AXIS2_PLACEMENT_3D('',#8839,#6883,#6884);
#5634=AXIS2_PLACEMENT_3D('',#8841,#6885,#6886);
#5635=AXIS2_PLACEMENT_3D('',#8842,#6887,#6888);
#5636=AXIS2_PLACEMENT_3D('',#8844,#6889,#6890);
#5637=AXIS2_PLACEMENT_3D('',#8845,#6891,#6892);
#5638=AXIS2_PLACEMENT_3D('',#8847,#6894,#6895);
#5639=AXIS2_PLACEMENT_3D('',#8849,#6896,#6897);
#5640=AXIS2_PLACEMENT_3D('',#8851,#6899,#6900);
#5641=AXIS2_PLACEMENT_3D('',#8854,#6902,#6903);
#5642=AXIS2_PLACEMENT_3D('',#8855,#6904,#6905);
#5643=AXIS2_PLACEMENT_3D('',#8857,#6906,#6907);
#5644=AXIS2_PLACEMENT_3D('',#8860,#6909,#6910);
#5645=AXIS2_PLACEMENT_3D('',#8861,#6911,#6912);
#5646=AXIS2_PLACEMENT_3D('',#8862,#6913,#6914);
#5647=AXIS2_PLACEMENT_3D('',#8910,#6916,#6917);
#5648=AXIS2_PLACEMENT_3D('',#8913,#6919,#6920);
#5649=AXIS2_PLACEMENT_3D('',#8914,#6921,#6922);
#5650=AXIS2_PLACEMENT_3D('',#8915,#6923,#6924);
#5651=AXIS2_PLACEMENT_3D('',#8916,#6925,#6926);
#5652=AXIS2_PLACEMENT_3D('',#8917,#6927,#6928);
#5653=AXIS2_PLACEMENT_3D('',#8918,#6929,#6930);
#5654=AXIS2_PLACEMENT_3D('',#8920,#6931,#6932);
#5655=AXIS2_PLACEMENT_3D('',#8923,#6934,#6935);
#5656=AXIS2_PLACEMENT_3D('',#8924,#6936,#6937);
#5657=AXIS2_PLACEMENT_3D('',#8926,#6938,#6939);
#5658=AXIS2_PLACEMENT_3D('',#8929,#6941,#6942);
#5659=AXIS2_PLACEMENT_3D('',#8930,#6943,#6944);
#5660=AXIS2_PLACEMENT_3D('',#8931,#6945,#6946);
#5661=AXIS2_PLACEMENT_3D('',#8932,#6947,#6948);
#5662=AXIS2_PLACEMENT_3D('',#8933,#6949,#6950);
#5663=AXIS2_PLACEMENT_3D('',#8937,#6952,#6953);
#5664=AXIS2_PLACEMENT_3D('',#8938,#6954,#6955);
#5665=AXIS2_PLACEMENT_3D('',#8955,#6956,#6957);
#5666=AXIS2_PLACEMENT_3D('',#8996,#6959,#6960);
#5667=AXIS2_PLACEMENT_3D('',#9011,#6961,#6962);
#5668=AXIS2_PLACEMENT_3D('',#9013,#6964,#6965);
#5669=AXIS2_PLACEMENT_3D('',#9015,#6966,#6967);
#5670=AXIS2_PLACEMENT_3D('',#9018,#6969,#6970);
#5671=AXIS2_PLACEMENT_3D('',#9019,#6971,#6972);
#5672=AXIS2_PLACEMENT_3D('',#9021,#6973,#6974);
#5673=AXIS2_PLACEMENT_3D('',#9024,#6976,#6977);
#5674=AXIS2_PLACEMENT_3D('',#9025,#6978,#6979);
#5675=AXIS2_PLACEMENT_3D('',#9026,#6980,#6981);
#5676=AXIS2_PLACEMENT_3D('',#9027,#6982,#6983);
#5677=AXIS2_PLACEMENT_3D('',#9028,#6984,#6985);
#5678=AXIS2_PLACEMENT_3D('',#9037,#6990,#6991);
#5679=AXIS2_PLACEMENT_3D('',#9043,#6995,#6996);
#5680=AXIS2_PLACEMENT_3D('',#9049,#7000,#7001);
#5681=AXIS2_PLACEMENT_3D('',#9051,#7002,#7003);
#5682=AXIS2_PLACEMENT_3D('',#9053,#7004,#7005);
#5683=AXIS2_PLACEMENT_3D('',#9055,#7006,#7007);
#5684=AXIS2_PLACEMENT_3D('',#9057,#7008,#7009);
#5685=AXIS2_PLACEMENT_3D('',#9059,#7010,#7011);
#5686=AXIS2_PLACEMENT_3D('',#9060,#7012,#7013);
#5687=AXIS2_PLACEMENT_3D('',#9061,#7014,#7015);
#5688=AXIS2_PLACEMENT_3D('',#9062,#7016,#7017);
#5689=AXIS2_PLACEMENT_3D('',#9063,#7018,#7019);
#5690=AXIS2_PLACEMENT_3D('',#9065,#7020,#7021);
#5691=AXIS2_PLACEMENT_3D('',#9067,#7023,#7024);
#5692=AXIS2_PLACEMENT_3D('',#9069,#7025,#7026);
#5693=AXIS2_PLACEMENT_3D('',#9071,#7028,#7029);
#5694=AXIS2_PLACEMENT_3D('',#9073,#7030,#7031);
#5695=AXIS2_PLACEMENT_3D('',#9075,#7033,#7034);
#5696=AXIS2_PLACEMENT_3D('',#9077,#7035,#7036);
#5697=AXIS2_PLACEMENT_3D('',#9079,#7038,#7039);
#5698=AXIS2_PLACEMENT_3D('',#9081,#7040,#7041);
#5699=AXIS2_PLACEMENT_3D('',#9083,#7042,#7043);
#5700=AXIS2_PLACEMENT_3D('',#9084,#7044,#7045);
#5701=AXIS2_PLACEMENT_3D('',#9086,#7047,#7048);
#5702=AXIS2_PLACEMENT_3D('',#9089,#7050,#7051);
#5703=AXIS2_PLACEMENT_3D('',#9090,#7052,#7053);
#5704=AXIS2_PLACEMENT_3D('',#9091,#7054,#7055);
#5705=AXIS2_PLACEMENT_3D('',#9092,#7056,#7057);
#5706=AXIS2_PLACEMENT_3D('',#9094,#7058,#7059);
#5707=AXIS2_PLACEMENT_3D('',#9097,#7061,#7062);
#5708=AXIS2_PLACEMENT_3D('',#9098,#7063,#7064);
#5709=AXIS2_PLACEMENT_3D('',#9100,#7065,#7066);
#5710=AXIS2_PLACEMENT_3D('',#9103,#7068,#7069);
#5711=AXIS2_PLACEMENT_3D('',#9104,#7070,#7071);
#5712=AXIS2_PLACEMENT_3D('',#9105,#7072,#7073);
#5713=AXIS2_PLACEMENT_3D('',#9106,#7074,#7075);
#5714=AXIS2_PLACEMENT_3D('',#9107,#7076,#7077);
#5715=AXIS2_PLACEMENT_3D('',#9121,#7084,#7085);
#5716=AXIS2_PLACEMENT_3D('',#9122,#7086,#7087);
#5717=AXIS2_PLACEMENT_3D('',#9136,#7094,#7095);
#5718=AXIS2_PLACEMENT_3D('',#9137,#7096,#7097);
#5719=AXIS2_PLACEMENT_3D('',#9140,#7100,#7101);
#5720=AXIS2_PLACEMENT_3D('',#9142,#7103,#7104);
#5721=AXIS2_PLACEMENT_3D('',#9144,#7106,#7107);
#5722=AXIS2_PLACEMENT_3D('',#9146,#7109,#7110);
#5723=AXIS2_PLACEMENT_3D('',#9148,#7112,#7113);
#5724=AXIS2_PLACEMENT_3D('',#9149,#7114,#7115);
#5725=AXIS2_PLACEMENT_3D('',#9152,#7117,#7118);
#5726=AXIS2_PLACEMENT_3D('',#9153,#7119,#7120);
#5727=AXIS2_PLACEMENT_3D('',#9155,#7121,#7122);
#5728=AXIS2_PLACEMENT_3D('',#9157,#7123,#7124);
#5729=AXIS2_PLACEMENT_3D('',#9158,#7125,#7126);
#5730=AXIS2_PLACEMENT_3D('',#9160,#7128,#7129);
#5731=AXIS2_PLACEMENT_3D('',#9162,#7130,#7131);
#5732=AXIS2_PLACEMENT_3D('',#9164,#7133,#7134);
#5733=AXIS2_PLACEMENT_3D('',#9166,#7135,#7136);
#5734=AXIS2_PLACEMENT_3D('',#9168,#7138,#7139);
#5735=AXIS2_PLACEMENT_3D('',#9170,#7140,#7141);
#5736=AXIS2_PLACEMENT_3D('',#9171,#7142,#7143);
#5737=AXIS2_PLACEMENT_3D('',#9173,#7145,#7146);
#5738=AXIS2_PLACEMENT_3D('',#9174,#7147,#7148);
#5739=AXIS2_PLACEMENT_3D('',#9175,#7149,#7150);
#5740=AXIS2_PLACEMENT_3D('',#9176,#7151,#7152);
#5741=AXIS2_PLACEMENT_3D('',#9177,#7153,#7154);
#5742=AXIS2_PLACEMENT_3D('',#9178,#7155,#7156);
#5743=AXIS2_PLACEMENT_3D('',#9179,#7157,#7158);
#5744=AXIS2_PLACEMENT_3D('',#9180,#7159,#7160);
#5745=AXIS2_PLACEMENT_3D('',#9181,#7161,#7162);
#5746=AXIS2_PLACEMENT_3D('',#9182,#7163,#7164);
#5747=AXIS2_PLACEMENT_3D('',#9183,#7165,#7166);
#5748=AXIS2_PLACEMENT_3D('',#9184,#7167,#7168);
#5749=AXIS2_PLACEMENT_3D('',#9185,#7169,#7170);
#5750=AXIS2_PLACEMENT_3D('',#9186,#7171,#7172);
#5751=AXIS2_PLACEMENT_3D('',#9187,#7173,#7174);
#5752=AXIS2_PLACEMENT_3D('',#9188,#7175,#7176);
#5753=AXIS2_PLACEMENT_3D('',#9189,#7177,#7178);
#5754=AXIS2_PLACEMENT_3D('',#9190,#7179,#7180);
#5755=AXIS2_PLACEMENT_3D('',#9191,#7181,#7182);
#5756=AXIS2_PLACEMENT_3D('',#9192,#7183,#7184);
#5757=AXIS2_PLACEMENT_3D('',#9193,#7185,#7186);
#5758=AXIS2_PLACEMENT_3D('',#9194,#7187,#7188);
#5759=AXIS2_PLACEMENT_3D('',#9195,#7189,#7190);
#5760=AXIS2_PLACEMENT_3D('',#9196,#7191,#7192);
#5761=AXIS2_PLACEMENT_3D('',#9197,#7193,#7194);
#5762=AXIS2_PLACEMENT_3D('',#9198,#7195,#7196);
#5763=AXIS2_PLACEMENT_3D('',#9199,#7197,#7198);
#5764=AXIS2_PLACEMENT_3D('',#9200,#7199,#7200);
#5765=AXIS2_PLACEMENT_3D('',#9209,#7205,#7206);
#5766=AXIS2_PLACEMENT_3D('',#9215,#7210,#7211);
#5767=AXIS2_PLACEMENT_3D('',#9221,#7215,#7216);
#5768=AXIS2_PLACEMENT_3D('',#9227,#7220,#7221);
#5769=AXIS2_PLACEMENT_3D('',#9233,#7225,#7226);
#5770=AXIS2_PLACEMENT_3D('',#9236,#7229,#7230);
#5771=AXIS2_PLACEMENT_3D('',#9237,#7231,#7232);
#5772=AXIS2_PLACEMENT_3D('',#9239,#7233,#7234);
#5773=AXIS2_PLACEMENT_3D('',#9240,#7235,#7236);
#5774=AXIS2_PLACEMENT_3D('',#9242,#7237,#7238);
#5775=AXIS2_PLACEMENT_3D('',#9244,#7240,#7241);
#5776=AXIS2_PLACEMENT_3D('',#9246,#7242,#7243);
#5777=AXIS2_PLACEMENT_3D('',#9248,#7245,#7246);
#5778=AXIS2_PLACEMENT_3D('',#9250,#7247,#7248);
#5779=AXIS2_PLACEMENT_3D('',#9252,#7250,#7251);
#5780=AXIS2_PLACEMENT_3D('',#9253,#7252,#7253);
#5781=AXIS2_PLACEMENT_3D('',#9254,#7254,#7255);
#5782=AXIS2_PLACEMENT_3D('',#9271,#7264,#7265);
#5783=AXIS2_PLACEMENT_3D('',#9277,#7269,#7270);
#5784=AXIS2_PLACEMENT_3D('',#9281,#7273,#7274);
#5785=AXIS2_PLACEMENT_3D('',#9285,#7277,#7278);
#5786=AXIS2_PLACEMENT_3D('',#9289,#7281,#7282);
#5787=AXIS2_PLACEMENT_3D('',#9297,#7287,#7288);
#5788=AXIS2_PLACEMENT_3D('',#9299,#7290,#7291);
#5789=AXIS2_PLACEMENT_3D('',#9301,#7293,#7294);
#5790=AXIS2_PLACEMENT_3D('',#9303,#7296,#7297);
#5791=AXIS2_PLACEMENT_3D('',#9304,#7298,#7299);
#5792=AXIS2_PLACEMENT_3D('',#9305,#7300,#7301);
#5793=AXIS2_PLACEMENT_3D('',#9307,#7302,#7303);
#5794=AXIS2_PLACEMENT_3D('',#9308,#7304,#7305);
#5795=AXIS2_PLACEMENT_3D('',#9310,#7306,#7307);
#5796=AXIS2_PLACEMENT_3D('',#9312,#7309,#7310);
#5797=AXIS2_PLACEMENT_3D('',#9314,#7311,#7312);
#5798=AXIS2_PLACEMENT_3D('',#9316,#7314,#7315);
#5799=AXIS2_PLACEMENT_3D('',#9318,#7316,#7317);
#5800=AXIS2_PLACEMENT_3D('',#9320,#7319,#7320);
#5801=AXIS2_PLACEMENT_3D('',#9322,#7321,#7322);
#5802=AXIS2_PLACEMENT_3D('',#9323,#7323,#7324);
#5803=AXIS2_PLACEMENT_3D('',#9325,#7325,#7326);
#5804=AXIS2_PLACEMENT_3D('',#9327,#7328,#7329);
#5805=AXIS2_PLACEMENT_3D('',#9329,#7330,#7331);
#5806=AXIS2_PLACEMENT_3D('',#9331,#7333,#7334);
#5807=AXIS2_PLACEMENT_3D('',#9333,#7335,#7336);
#5808=AXIS2_PLACEMENT_3D('',#9335,#7338,#7339);
#5809=AXIS2_PLACEMENT_3D('',#9336,#7340,#7341);
#5810=AXIS2_PLACEMENT_3D('',#9345,#7346,#7347);
#5811=AXIS2_PLACEMENT_3D('',#9351,#7351,#7352);
#5812=AXIS2_PLACEMENT_3D('',#9357,#7356,#7357);
#5813=AXIS2_PLACEMENT_3D('',#9363,#7361,#7362);
#5814=AXIS2_PLACEMENT_3D('',#9369,#7366,#7367);
#5815=AXIS2_PLACEMENT_3D('',#9372,#7370,#7371);
#5816=AXIS2_PLACEMENT_3D('',#9373,#7372,#7373);
#5817=AXIS2_PLACEMENT_3D('',#9374,#7374,#7375);
#5818=AXIS2_PLACEMENT_3D('',#9375,#7376,#7377);
#5819=AXIS2_PLACEMENT_3D('',#9376,#7378,#7379);
#5820=AXIS2_PLACEMENT_3D('',#9377,#7380,#7381);
#5821=AXIS2_PLACEMENT_3D('',#9378,#7382,#7383);
#5822=AXIS2_PLACEMENT_3D('',#9379,#7384,#7385);
#5823=AXIS2_PLACEMENT_3D('',#9380,#7386,#7387);
#5824=AXIS2_PLACEMENT_3D('',#9381,#7388,#7389);
#5825=AXIS2_PLACEMENT_3D('',#9382,#7390,#7391);
#5826=AXIS2_PLACEMENT_3D('',#9383,#7392,#7393);
#5827=AXIS2_PLACEMENT_3D('',#9384,#7394,#7395);
#5828=DIRECTION('axis',(0.,0.,1.));
#5829=DIRECTION('refdir',(1.,0.,0.));
#5830=DIRECTION('axis',(0.,0.,1.));
#5831=DIRECTION('refdir',(1.,0.,0.));
#5832=DIRECTION('axis',(0.,0.,1.));
#5833=DIRECTION('refdir',(1.,0.,0.));
#5834=DIRECTION('center_axis',(0.,0.,1.));
#5835=DIRECTION('ref_axis',(1.,0.,0.));
#5836=DIRECTION('center_axis',(0.,0.,1.));
#5837=DIRECTION('ref_axis',(1.,0.,0.));
#5838=DIRECTION('',(0.,0.,1.));
#5839=DIRECTION('center_axis',(0.,0.,-1.));
#5840=DIRECTION('ref_axis',(1.,0.,0.));
#5841=DIRECTION('center_axis',(0.,0.,1.));
#5842=DIRECTION('ref_axis',(1.,0.,0.));
#5843=DIRECTION('center_axis',(0.,0.,1.));
#5844=DIRECTION('ref_axis',(1.,0.,0.));
#5845=DIRECTION('',(0.,0.,1.));
#5846=DIRECTION('center_axis',(0.,0.,-1.));
#5847=DIRECTION('ref_axis',(1.,0.,0.));
#5848=DIRECTION('center_axis',(0.,0.,1.));
#5849=DIRECTION('ref_axis',(1.,0.,0.));
#5850=DIRECTION('center_axis',(0.,0.,1.));
#5851=DIRECTION('ref_axis',(1.,0.,0.));
#5852=DIRECTION('',(0.,0.,1.));
#5853=DIRECTION('center_axis',(0.,0.,-1.));
#5854=DIRECTION('ref_axis',(1.,0.,0.));
#5855=DIRECTION('center_axis',(0.,0.,1.));
#5856=DIRECTION('ref_axis',(1.,0.,0.));
#5857=DIRECTION('center_axis',(0.,0.,1.));
#5858=DIRECTION('ref_axis',(1.,0.,0.));
#5859=DIRECTION('',(0.,0.,1.));
#5860=DIRECTION('center_axis',(0.,0.,-1.));
#5861=DIRECTION('ref_axis',(1.,0.,0.));
#5862=DIRECTION('center_axis',(0.,1.,0.));
#5863=DIRECTION('ref_axis',(-1.,0.,0.));
#5864=DIRECTION('',(-1.,0.,0.));
#5865=DIRECTION('',(0.,0.,1.));
#5866=DIRECTION('',(-1.,0.,0.));
#5867=DIRECTION('',(0.,0.,1.));
#5868=DIRECTION('center_axis',(1.,0.,0.));
#5869=DIRECTION('ref_axis',(0.,1.,0.));
#5870=DIRECTION('',(0.,1.,0.));
#5871=DIRECTION('',(0.,1.,0.));
#5872=DIRECTION('',(0.,0.,1.));
#5873=DIRECTION('center_axis',(0.,-1.,0.));
#5874=DIRECTION('ref_axis',(1.,0.,0.));
#5875=DIRECTION('',(1.,0.,0.));
#5876=DIRECTION('',(1.,0.,0.));
#5877=DIRECTION('',(0.,0.,1.));
#5878=DIRECTION('center_axis',(-1.,0.,0.));
#5879=DIRECTION('ref_axis',(0.,-1.,0.));
#5880=DIRECTION('',(0.,-1.,0.));
#5881=DIRECTION('',(0.,-1.,0.));
#5882=DIRECTION('center_axis',(0.,0.,1.));
#5883=DIRECTION('ref_axis',(1.,0.,0.));
#5884=DIRECTION('center_axis',(0.,0.,1.));
#5885=DIRECTION('ref_axis',(1.,0.,0.));
#5886=DIRECTION('axis',(0.,0.,1.));
#5887=DIRECTION('refdir',(1.,0.,0.));
#5888=DIRECTION('center_axis',(0.,1.,0.));
#5889=DIRECTION('ref_axis',(1.,0.,0.));
#5890=DIRECTION('center_axis',(0.,1.,0.));
#5891=DIRECTION('ref_axis',(1.,0.,0.));
#5892=DIRECTION('',(0.,1.,0.));
#5893=DIRECTION('center_axis',(0.,-1.,0.));
#5894=DIRECTION('ref_axis',(1.,0.,0.));
#5895=DIRECTION('center_axis',(0.,1.,0.));
#5896=DIRECTION('ref_axis',(1.,0.,0.));
#5897=DIRECTION('center_axis',(0.,1.,0.));
#5898=DIRECTION('ref_axis',(1.,0.,0.));
#5899=DIRECTION('center_axis',(0.,1.,0.));
#5900=DIRECTION('ref_axis',(1.,0.,0.));
#5901=DIRECTION('',(0.,1.,0.));
#5902=DIRECTION('center_axis',(0.,-1.,0.));
#5903=DIRECTION('ref_axis',(1.,0.,0.));
#5904=DIRECTION('center_axis',(0.,1.,0.));
#5905=DIRECTION('ref_axis',(1.,0.,0.));
#5906=DIRECTION('center_axis',(0.,1.,0.));
#5907=DIRECTION('ref_axis',(1.,0.,0.));
#5908=DIRECTION('center_axis',(0.,1.,0.));
#5909=DIRECTION('ref_axis',(1.,0.,0.));
#5910=DIRECTION('',(0.,1.,0.));
#5911=DIRECTION('center_axis',(0.,-1.,0.));
#5912=DIRECTION('ref_axis',(1.,0.,0.));
#5913=DIRECTION('center_axis',(0.,1.,0.));
#5914=DIRECTION('ref_axis',(1.,0.,0.));
#5915=DIRECTION('center_axis',(0.,1.,0.));
#5916=DIRECTION('ref_axis',(1.,0.,0.));
#5917=DIRECTION('center_axis',(0.,1.,0.));
#5918=DIRECTION('ref_axis',(1.,0.,0.));
#5919=DIRECTION('',(0.,1.,0.));
#5920=DIRECTION('center_axis',(0.,-1.,0.));
#5921=DIRECTION('ref_axis',(1.,0.,0.));
#5922=DIRECTION('center_axis',(0.,1.,0.));
#5923=DIRECTION('ref_axis',(1.,0.,0.));
#5924=DIRECTION('center_axis',(0.,1.,0.));
#5925=DIRECTION('ref_axis',(1.,0.,0.));
#5926=DIRECTION('center_axis',(0.,1.,0.));
#5927=DIRECTION('ref_axis',(1.,0.,0.));
#5928=DIRECTION('',(0.,1.,0.));
#5929=DIRECTION('center_axis',(0.,1.,0.));
#5930=DIRECTION('ref_axis',(1.,0.,0.));
#5931=DIRECTION('center_axis',(0.,1.,0.));
#5932=DIRECTION('ref_axis',(1.,0.,0.));
#5933=DIRECTION('center_axis',(0.,1.,0.));
#5934=DIRECTION('ref_axis',(1.,0.,0.));
#5935=DIRECTION('center_axis',(0.,1.,0.));
#5936=DIRECTION('ref_axis',(1.,0.,0.));
#5937=DIRECTION('',(0.,1.,0.));
#5938=DIRECTION('center_axis',(0.,1.,0.));
#5939=DIRECTION('ref_axis',(1.,0.,0.));
#5940=DIRECTION('center_axis',(0.,1.,0.));
#5941=DIRECTION('ref_axis',(1.,0.,0.));
#5942=DIRECTION('center_axis',(0.,1.,0.));
#5943=DIRECTION('ref_axis',(1.,0.,0.));
#5944=DIRECTION('center_axis',(0.,1.,0.));
#5945=DIRECTION('ref_axis',(1.,0.,0.));
#5946=DIRECTION('',(0.,1.,0.));
#5947=DIRECTION('center_axis',(0.,1.,0.));
#5948=DIRECTION('ref_axis',(1.,0.,0.));
#5949=DIRECTION('center_axis',(0.,1.,0.));
#5950=DIRECTION('ref_axis',(1.,0.,0.));
#5951=DIRECTION('center_axis',(0.,1.,0.));
#5952=DIRECTION('ref_axis',(1.,0.,0.));
#5953=DIRECTION('center_axis',(0.,1.,0.));
#5954=DIRECTION('ref_axis',(1.,0.,0.));
#5955=DIRECTION('',(0.,1.,0.));
#5956=DIRECTION('center_axis',(0.,1.,0.));
#5957=DIRECTION('ref_axis',(1.,0.,0.));
#5958=DIRECTION('center_axis',(0.,1.,0.));
#5959=DIRECTION('ref_axis',(1.,0.,0.));
#5960=DIRECTION('center_axis',(1.,0.,0.));
#5961=DIRECTION('ref_axis',(0.,0.,-1.));
#5962=DIRECTION('',(1.,0.,0.));
#5963=DIRECTION('center_axis',(0.,0.,1.));
#5964=DIRECTION('ref_axis',(1.,0.,0.));
#5965=DIRECTION('center_axis',(0.,0.,1.));
#5966=DIRECTION('ref_axis',(1.,0.,0.));
#5967=DIRECTION('',(0.,0.,1.));
#5968=DIRECTION('center_axis',(0.,0.,-1.));
#5969=DIRECTION('ref_axis',(1.,0.,0.));
#5970=DIRECTION('center_axis',(0.,0.,1.));
#5971=DIRECTION('ref_axis',(1.,0.,0.));
#5972=DIRECTION('center_axis',(0.,0.,1.));
#5973=DIRECTION('ref_axis',(1.,0.,0.));
#5974=DIRECTION('',(0.,0.,1.));
#5975=DIRECTION('center_axis',(0.,0.,-1.));
#5976=DIRECTION('ref_axis',(1.,0.,0.));
#5977=DIRECTION('center_axis',(0.,0.,1.));
#5978=DIRECTION('ref_axis',(1.,0.,0.));
#5979=DIRECTION('center_axis',(0.,0.,1.));
#5980=DIRECTION('ref_axis',(1.,0.,0.));
#5981=DIRECTION('',(0.,0.,1.));
#5982=DIRECTION('center_axis',(0.,0.,-1.));
#5983=DIRECTION('ref_axis',(1.,0.,0.));
#5984=DIRECTION('center_axis',(0.,0.,1.));
#5985=DIRECTION('ref_axis',(1.,0.,0.));
#5986=DIRECTION('center_axis',(0.,0.,1.));
#5987=DIRECTION('ref_axis',(1.,0.,0.));
#5988=DIRECTION('',(0.,0.,1.));
#5989=DIRECTION('center_axis',(0.,0.,-1.));
#5990=DIRECTION('ref_axis',(1.,0.,0.));
#5991=DIRECTION('center_axis',(0.,1.,0.));
#5992=DIRECTION('ref_axis',(0.,0.,1.));
#5993=DIRECTION('center_axis',(0.,1.,0.));
#5994=DIRECTION('ref_axis',(1.,0.,0.));
#5995=DIRECTION('',(1.,0.,0.));
#5996=DIRECTION('',(0.,0.,-1.));
#5997=DIRECTION('',(-1.,0.,0.));
#5998=DIRECTION('center_axis',(0.,1.,0.));
#5999=DIRECTION('ref_axis',(0.,0.,1.));
#6000=DIRECTION('center_axis',(0.,1.,0.));
#6001=DIRECTION('ref_axis',(1.,0.,0.));
#6002=DIRECTION('',(-1.,0.,0.));
#6003=DIRECTION('',(0.,0.,1.));
#6004=DIRECTION('',(1.,0.,0.));
#6005=DIRECTION('center_axis',(0.,1.,0.));
#6006=DIRECTION('ref_axis',(1.,0.,0.));
#6007=DIRECTION('center_axis',(0.,-1.,0.));
#6008=DIRECTION('ref_axis',(1.,0.,0.));
#6009=DIRECTION('',(1.,0.,0.));
#6010=DIRECTION('',(0.,0.,1.));
#6011=DIRECTION('',(-1.,0.,0.));
#6012=DIRECTION('center_axis',(0.,1.,0.));
#6013=DIRECTION('ref_axis',(1.,0.,0.));
#6014=DIRECTION('center_axis',(0.,-1.,0.));
#6015=DIRECTION('ref_axis',(1.,0.,0.));
#6016=DIRECTION('',(-1.,0.,0.));
#6017=DIRECTION('',(0.,0.,-1.));
#6018=DIRECTION('',(1.,0.,0.));
#6019=DIRECTION('center_axis',(0.,0.,1.));
#6020=DIRECTION('ref_axis',(1.,0.,0.));
#6021=DIRECTION('',(0.,1.,0.));
#6022=DIRECTION('',(0.,1.,0.));
#6023=DIRECTION('center_axis',(0.,0.,1.));
#6024=DIRECTION('ref_axis',(1.,0.,0.));
#6025=DIRECTION('',(0.,-1.,0.));
#6026=DIRECTION('',(0.,1.,0.));
#6027=DIRECTION('center_axis',(-1.,0.,0.));
#6028=DIRECTION('ref_axis',(0.,0.,1.));
#6029=DIRECTION('',(0.,1.,0.));
#6030=DIRECTION('center_axis',(0.,0.,-1.));
#6031=DIRECTION('ref_axis',(-1.,0.,0.));
#6032=DIRECTION('',(0.,1.,0.));
#6033=DIRECTION('center_axis',(1.,0.,0.));
#6034=DIRECTION('ref_axis',(0.,0.,-1.));
#6035=DIRECTION('center_axis',(0.,1.,0.));
#6036=DIRECTION('ref_axis',(0.,0.,1.));
#6037=DIRECTION('center_axis',(0.,1.,0.));
#6038=DIRECTION('ref_axis',(1.,0.,0.));
#6039=DIRECTION('',(1.,0.,0.));
#6040=DIRECTION('',(0.,0.,-1.));
#6041=DIRECTION('',(-1.,0.,0.));
#6042=DIRECTION('center_axis',(0.,1.,0.));
#6043=DIRECTION('ref_axis',(0.,0.,1.));
#6044=DIRECTION('center_axis',(0.,1.,0.));
#6045=DIRECTION('ref_axis',(1.,0.,0.));
#6046=DIRECTION('',(-1.,0.,0.));
#6047=DIRECTION('',(0.,0.,1.));
#6048=DIRECTION('',(1.,0.,0.));
#6049=DIRECTION('center_axis',(0.,1.,0.));
#6050=DIRECTION('ref_axis',(1.,0.,0.));
#6051=DIRECTION('center_axis',(0.,-1.,0.));
#6052=DIRECTION('ref_axis',(1.,0.,0.));
#6053=DIRECTION('',(1.,0.,0.));
#6054=DIRECTION('',(0.,0.,1.));
#6055=DIRECTION('',(-1.,0.,0.));
#6056=DIRECTION('center_axis',(0.,1.,0.));
#6057=DIRECTION('ref_axis',(1.,0.,0.));
#6058=DIRECTION('center_axis',(0.,-1.,0.));
#6059=DIRECTION('ref_axis',(1.,0.,0.));
#6060=DIRECTION('',(-1.,0.,0.));
#6061=DIRECTION('',(0.,0.,-1.));
#6062=DIRECTION('',(1.,0.,0.));
#6063=DIRECTION('center_axis',(0.,0.,1.));
#6064=DIRECTION('ref_axis',(1.,0.,0.));
#6065=DIRECTION('',(0.,1.,0.));
#6066=DIRECTION('',(0.,1.,0.));
#6067=DIRECTION('center_axis',(0.,0.,1.));
#6068=DIRECTION('ref_axis',(1.,0.,0.));
#6069=DIRECTION('',(0.,-1.,0.));
#6070=DIRECTION('',(0.,1.,0.));
#6071=DIRECTION('center_axis',(-1.,0.,0.));
#6072=DIRECTION('ref_axis',(0.,0.,1.));
#6073=DIRECTION('',(0.,1.,0.));
#6074=DIRECTION('center_axis',(0.,0.,-1.));
#6075=DIRECTION('ref_axis',(-1.,0.,0.));
#6076=DIRECTION('',(0.,1.,0.));
#6077=DIRECTION('center_axis',(1.,0.,0.));
#6078=DIRECTION('ref_axis',(0.,0.,-1.));
#6079=DIRECTION('center_axis',(0.,1.,0.));
#6080=DIRECTION('ref_axis',(1.,0.,0.));
#6081=DIRECTION('center_axis',(0.,-1.,0.));
#6082=DIRECTION('ref_axis',(1.,0.,0.));
#6083=DIRECTION('',(0.,-1.,0.));
#6084=DIRECTION('center_axis',(0.,-1.,0.));
#6085=DIRECTION('ref_axis',(1.,0.,0.));
#6086=DIRECTION('center_axis',(0.,1.,0.));
#6087=DIRECTION('ref_axis',(1.,0.,0.));
#6088=DIRECTION('center_axis',(0.,1.,0.));
#6089=DIRECTION('ref_axis',(1.,0.,0.));
#6090=DIRECTION('',(0.,-1.,0.));
#6091=DIRECTION('center_axis',(0.,1.,0.));
#6092=DIRECTION('ref_axis',(1.,0.,0.));
#6093=DIRECTION('center_axis',(0.,1.,0.));
#6094=DIRECTION('ref_axis',(1.,0.,0.));
#6095=DIRECTION('center_axis',(0.,1.,0.));
#6096=DIRECTION('ref_axis',(1.,0.,0.));
#6097=DIRECTION('axis',(0.,0.,1.));
#6098=DIRECTION('refdir',(1.,0.,0.));
#6099=DIRECTION('center_axis',(0.,1.,0.));
#6100=DIRECTION('ref_axis',(1.,0.,0.));
#6101=DIRECTION('center_axis',(0.,1.,0.));
#6102=DIRECTION('ref_axis',(1.,0.,0.));
#6103=DIRECTION('',(0.,1.,0.));
#6104=DIRECTION('center_axis',(0.,1.,0.));
#6105=DIRECTION('ref_axis',(1.,0.,0.));
#6106=DIRECTION('center_axis',(0.,1.,0.));
#6107=DIRECTION('ref_axis',(1.,0.,0.));
#6108=DIRECTION('center_axis',(0.,-1.,0.));
#6109=DIRECTION('ref_axis',(1.,0.,0.));
#6110=DIRECTION('center_axis',(0.,1.,0.));
#6111=DIRECTION('ref_axis',(1.,0.,0.));
#6112=DIRECTION('center_axis',(0.,1.,0.));
#6113=DIRECTION('ref_axis',(1.,0.,0.));
#6114=DIRECTION('center_axis',(0.,1.,0.));
#6115=DIRECTION('ref_axis',(1.,0.,0.));
#6116=DIRECTION('',(0.,-1.,0.));
#6117=DIRECTION('center_axis',(0.,-1.,0.));
#6118=DIRECTION('ref_axis',(1.,0.,0.));
#6119=DIRECTION('center_axis',(0.,1.,0.));
#6120=DIRECTION('ref_axis',(1.,0.,0.));
#6121=DIRECTION('center_axis',(0.,-1.,0.));
#6122=DIRECTION('ref_axis',(1.,0.,0.));
#6123=DIRECTION('',(0.,-1.,0.));
#6124=DIRECTION('center_axis',(0.,1.,0.));
#6125=DIRECTION('ref_axis',(1.,0.,0.));
#6126=DIRECTION('center_axis',(0.,1.,0.));
#6127=DIRECTION('ref_axis',(1.,0.,0.));
#6128=DIRECTION('',(0.,-1.,0.));
#6129=DIRECTION('center_axis',(0.,1.,0.));
#6130=DIRECTION('ref_axis',(1.,0.,0.));
#6131=DIRECTION('center_axis',(0.,1.,0.));
#6132=DIRECTION('ref_axis',(1.,0.,0.));
#6133=DIRECTION('center_axis',(0.,1.,0.));
#6134=DIRECTION('ref_axis',(1.,0.,0.));
#6135=DIRECTION('axis',(0.,0.,1.));
#6136=DIRECTION('refdir',(1.,0.,0.));
#6137=DIRECTION('center_axis',(0.,-1.,0.));
#6138=DIRECTION('ref_axis',(0.,0.,-1.));
#6139=DIRECTION('center_axis',(-1.,0.,-1.22464679914735E-16));
#6140=DIRECTION('ref_axis',(-1.22464679914735E-16,0.,1.));
#6141=DIRECTION('center_axis',(0.,1.,0.));
#6142=DIRECTION('ref_axis',(0.,0.,-1.));
#6143=DIRECTION('axis',(0.,0.,1.));
#6144=DIRECTION('refdir',(1.,0.,0.));
#6145=DIRECTION('center_axis',(0.,1.,0.));
#6146=DIRECTION('ref_axis',(1.,0.,0.));
#6147=DIRECTION('center_axis',(0.,1.,0.));
#6148=DIRECTION('ref_axis',(1.,0.,0.));
#6149=DIRECTION('',(0.,1.,0.));
#6150=DIRECTION('center_axis',(0.,1.,0.));
#6151=DIRECTION('ref_axis',(1.,0.,0.));
#6152=DIRECTION('center_axis',(0.,1.,0.));
#6153=DIRECTION('ref_axis',(1.,0.,0.));
#6154=DIRECTION('center_axis',(0.,-1.,0.));
#6155=DIRECTION('ref_axis',(1.,0.,0.));
#6156=DIRECTION('center_axis',(0.,1.,0.));
#6157=DIRECTION('ref_axis',(1.,0.,0.));
#6158=DIRECTION('center_axis',(0.,1.,0.));
#6159=DIRECTION('ref_axis',(1.,0.,0.));
#6160=DIRECTION('center_axis',(0.,1.,0.));
#6161=DIRECTION('ref_axis',(1.,0.,0.));
#6162=DIRECTION('',(0.,-1.,0.));
#6163=DIRECTION('center_axis',(0.,-1.,0.));
#6164=DIRECTION('ref_axis',(1.,0.,0.));
#6165=DIRECTION('center_axis',(0.,1.,0.));
#6166=DIRECTION('ref_axis',(1.,0.,0.));
#6167=DIRECTION('center_axis',(0.,-1.,0.));
#6168=DIRECTION('ref_axis',(1.,0.,0.));
#6169=DIRECTION('',(0.,-1.,0.));
#6170=DIRECTION('center_axis',(0.,1.,0.));
#6171=DIRECTION('ref_axis',(1.,0.,0.));
#6172=DIRECTION('center_axis',(0.,1.,0.));
#6173=DIRECTION('ref_axis',(1.,0.,0.));
#6174=DIRECTION('',(0.,-1.,0.));
#6175=DIRECTION('center_axis',(0.,1.,0.));
#6176=DIRECTION('ref_axis',(1.,0.,0.));
#6177=DIRECTION('center_axis',(0.,1.,0.));
#6178=DIRECTION('ref_axis',(1.,0.,0.));
#6179=DIRECTION('center_axis',(0.,1.,0.));
#6180=DIRECTION('ref_axis',(1.,0.,0.));
#6181=DIRECTION('axis',(0.,0.,1.));
#6182=DIRECTION('refdir',(1.,0.,0.));
#6183=DIRECTION('center_axis',(0.,-1.,0.));
#6184=DIRECTION('ref_axis',(0.,0.,-1.));
#6185=DIRECTION('center_axis',(-1.,0.,-1.22464679914735E-16));
#6186=DIRECTION('ref_axis',(-1.22464679914735E-16,0.,1.));
#6187=DIRECTION('center_axis',(0.,1.,0.));
#6188=DIRECTION('ref_axis',(0.,0.,-1.));
#6189=DIRECTION('axis',(0.,0.,1.));
#6190=DIRECTION('refdir',(1.,0.,0.));
#6191=DIRECTION('center_axis',(1.,0.,0.));
#6192=DIRECTION('ref_axis',(0.,0.,-1.));
#6193=DIRECTION('',(-1.,0.,0.));
#6194=DIRECTION('',(1.,0.,0.));
#6195=DIRECTION('center_axis',(1.,0.,0.));
#6196=DIRECTION('ref_axis',(0.,0.,-1.));
#6197=DIRECTION('center_axis',(1.,0.,0.));
#6198=DIRECTION('ref_axis',(0.,7.6571373978539E-16,1.));
#6199=DIRECTION('',(1.,0.,0.));
#6200=DIRECTION('center_axis',(1.,0.,0.));
#6201=DIRECTION('ref_axis',(0.,0.,-1.));
#6202=DIRECTION('',(-1.,0.,0.));
#6203=DIRECTION('center_axis',(1.,0.,0.));
#6204=DIRECTION('ref_axis',(0.,0.,-1.));
#6205=DIRECTION('',(0.,0.,1.));
#6206=DIRECTION('',(0.,0.,-1.));
#6207=DIRECTION('center_axis',(1.,0.,0.));
#6208=DIRECTION('ref_axis',(0.,0.,-1.));
#6209=DIRECTION('center_axis',(0.,1.,0.));
#6210=DIRECTION('ref_axis',(1.,0.,0.));
#6211=DIRECTION('center_axis',(0.,1.,0.));
#6212=DIRECTION('ref_axis',(1.,0.,0.));
#6213=DIRECTION('center_axis',(0.,-1.,0.));
#6214=DIRECTION('ref_axis',(1.,0.,0.));
#6215=DIRECTION('center_axis',(0.,1.,0.));
#6216=DIRECTION('ref_axis',(-1.,0.,1.22464679914735E-16));
#6217=DIRECTION('center_axis',(0.,1.,0.));
#6218=DIRECTION('ref_axis',(1.,0.,0.));
#6219=DIRECTION('center_axis',(1.,0.,0.));
#6220=DIRECTION('ref_axis',(0.,0.,-1.));
#6221=DIRECTION('',(1.,0.,0.));
#6222=DIRECTION('center_axis',(0.,1.,0.));
#6223=DIRECTION('ref_axis',(1.,0.,0.));
#6224=DIRECTION('',(0.,-1.,0.));
#6225=DIRECTION('center_axis',(0.,-1.,0.));
#6226=DIRECTION('ref_axis',(1.,0.,0.));
#6227=DIRECTION('center_axis',(0.,1.,0.));
#6228=DIRECTION('ref_axis',(1.,0.,0.));
#6229=DIRECTION('axis',(0.,0.,1.));
#6230=DIRECTION('refdir',(1.,0.,0.));
#6231=DIRECTION('center_axis',(0.,1.,0.));
#6232=DIRECTION('ref_axis',(1.,0.,0.));
#6233=DIRECTION('center_axis',(0.,1.,0.));
#6234=DIRECTION('ref_axis',(1.,0.,0.));
#6235=DIRECTION('',(0.,1.,0.));
#6236=DIRECTION('center_axis',(0.,-1.,0.));
#6237=DIRECTION('ref_axis',(1.,0.,0.));
#6238=DIRECTION('center_axis',(0.,1.,0.));
#6239=DIRECTION('ref_axis',(1.,0.,0.));
#6240=DIRECTION('center_axis',(0.,1.,0.));
#6241=DIRECTION('ref_axis',(1.,0.,0.));
#6242=DIRECTION('',(0.,1.,0.));
#6243=DIRECTION('center_axis',(0.,-1.,0.));
#6244=DIRECTION('ref_axis',(1.,0.,0.));
#6245=DIRECTION('center_axis',(0.,1.,0.));
#6246=DIRECTION('ref_axis',(1.,0.,0.));
#6247=DIRECTION('center_axis',(0.,1.,0.));
#6248=DIRECTION('ref_axis',(1.,0.,0.));
#6249=DIRECTION('',(0.,1.,0.));
#6250=DIRECTION('center_axis',(0.,-1.,0.));
#6251=DIRECTION('ref_axis',(1.,0.,0.));
#6252=DIRECTION('center_axis',(0.,1.,0.));
#6253=DIRECTION('ref_axis',(1.,0.,0.));
#6254=DIRECTION('center_axis',(0.,1.,0.));
#6255=DIRECTION('ref_axis',(1.,0.,0.));
#6256=DIRECTION('',(0.,1.,0.));
#6257=DIRECTION('center_axis',(0.,-1.,0.));
#6258=DIRECTION('ref_axis',(1.,0.,0.));
#6259=DIRECTION('center_axis',(0.,1.,0.));
#6260=DIRECTION('ref_axis',(1.,0.,0.));
#6261=DIRECTION('center_axis',(0.,1.,0.));
#6262=DIRECTION('ref_axis',(1.,0.,0.));
#6263=DIRECTION('',(0.,-1.,0.));
#6264=DIRECTION('center_axis',(0.,-1.,0.));
#6265=DIRECTION('ref_axis',(1.,0.,0.));
#6266=DIRECTION('center_axis',(0.,1.,0.));
#6267=DIRECTION('ref_axis',(1.,0.,0.));
#6268=DIRECTION('center_axis',(0.,-1.,0.));
#6269=DIRECTION('ref_axis',(1.,0.,0.));
#6270=DIRECTION('center_axis',(0.,1.,0.));
#6271=DIRECTION('ref_axis',(1.,0.,0.));
#6272=DIRECTION('',(0.,-1.,0.));
#6273=DIRECTION('center_axis',(0.,-1.,0.));
#6274=DIRECTION('ref_axis',(1.,0.,0.));
#6275=DIRECTION('center_axis',(0.,1.,0.));
#6276=DIRECTION('ref_axis',(1.,0.,0.));
#6277=DIRECTION('center_axis',(0.,1.,0.));
#6278=DIRECTION('ref_axis',(1.,0.,0.));
#6279=DIRECTION('',(0.,-1.,0.));
#6280=DIRECTION('center_axis',(0.,1.,0.));
#6281=DIRECTION('ref_axis',(1.,0.,0.));
#6282=DIRECTION('center_axis',(0.,1.,0.));
#6283=DIRECTION('ref_axis',(1.,0.,0.));
#6284=DIRECTION('center_axis',(0.,1.,0.));
#6285=DIRECTION('ref_axis',(1.,0.,0.));
#6286=DIRECTION('axis',(0.,0.,1.));
#6287=DIRECTION('refdir',(1.,0.,0.));
#6288=DIRECTION('center_axis',(0.,1.,0.));
#6289=DIRECTION('ref_axis',(1.,0.,0.));
#6290=DIRECTION('center_axis',(0.,1.,0.));
#6291=DIRECTION('ref_axis',(1.,0.,0.));
#6292=DIRECTION('',(0.,1.,0.));
#6293=DIRECTION('center_axis',(0.,-1.,0.));
#6294=DIRECTION('ref_axis',(1.,0.,0.));
#6295=DIRECTION('center_axis',(0.,1.,0.));
#6296=DIRECTION('ref_axis',(1.,0.,0.));
#6297=DIRECTION('center_axis',(0.,1.,0.));
#6298=DIRECTION('ref_axis',(1.,0.,0.));
#6299=DIRECTION('',(0.,1.,0.));
#6300=DIRECTION('center_axis',(0.,-1.,0.));
#6301=DIRECTION('ref_axis',(1.,0.,0.));
#6302=DIRECTION('center_axis',(0.,1.,0.));
#6303=DIRECTION('ref_axis',(1.,0.,0.));
#6304=DIRECTION('center_axis',(0.,1.,0.));
#6305=DIRECTION('ref_axis',(1.,0.,0.));
#6306=DIRECTION('',(0.,1.,0.));
#6307=DIRECTION('center_axis',(0.,-1.,0.));
#6308=DIRECTION('ref_axis',(1.,0.,0.));
#6309=DIRECTION('center_axis',(0.,1.,0.));
#6310=DIRECTION('ref_axis',(1.,0.,0.));
#6311=DIRECTION('center_axis',(0.,1.,0.));
#6312=DIRECTION('ref_axis',(1.,0.,0.));
#6313=DIRECTION('',(0.,1.,0.));
#6314=DIRECTION('center_axis',(0.,-1.,0.));
#6315=DIRECTION('ref_axis',(1.,0.,0.));
#6316=DIRECTION('center_axis',(0.,1.,0.));
#6317=DIRECTION('ref_axis',(1.,0.,0.));
#6318=DIRECTION('center_axis',(0.,1.,0.));
#6319=DIRECTION('ref_axis',(1.,0.,0.));
#6320=DIRECTION('',(0.,-1.,0.));
#6321=DIRECTION('center_axis',(0.,1.,0.));
#6322=DIRECTION('ref_axis',(1.,0.,0.));
#6323=DIRECTION('center_axis',(0.,1.,0.));
#6324=DIRECTION('ref_axis',(1.,0.,0.));
#6325=DIRECTION('center_axis',(0.,-1.,0.));
#6326=DIRECTION('ref_axis',(1.,0.,0.));
#6327=DIRECTION('center_axis',(0.,1.,0.));
#6328=DIRECTION('ref_axis',(1.,0.,0.));
#6329=DIRECTION('center_axis',(0.,-1.,0.));
#6330=DIRECTION('ref_axis',(1.,0.,0.));
#6331=DIRECTION('',(0.,-1.,0.));
#6332=DIRECTION('center_axis',(0.,1.,0.));
#6333=DIRECTION('ref_axis',(1.,0.,0.));
#6334=DIRECTION('center_axis',(0.,1.,0.));
#6335=DIRECTION('ref_axis',(1.,0.,0.));
#6336=DIRECTION('',(0.,-1.,0.));
#6337=DIRECTION('center_axis',(0.,1.,0.));
#6338=DIRECTION('ref_axis',(1.,0.,0.));
#6339=DIRECTION('center_axis',(0.,1.,0.));
#6340=DIRECTION('ref_axis',(1.,0.,0.));
#6341=DIRECTION('center_axis',(0.,1.,0.));
#6342=DIRECTION('ref_axis',(1.,0.,0.));
#6343=DIRECTION('axis',(0.,0.,1.));
#6344=DIRECTION('refdir',(1.,0.,0.));
#6345=DIRECTION('center_axis',(0.,1.,0.));
#6346=DIRECTION('ref_axis',(-1.,0.,0.));
#6347=DIRECTION('',(-1.,0.,0.));
#6348=DIRECTION('',(0.,0.,1.));
#6349=DIRECTION('',(-1.,0.,0.));
#6350=DIRECTION('',(0.,0.,1.));
#6351=DIRECTION('center_axis',(1.,0.,0.));
#6352=DIRECTION('ref_axis',(0.,1.,0.));
#6353=DIRECTION('',(0.,1.,0.));
#6354=DIRECTION('',(0.,1.,0.));
#6355=DIRECTION('',(0.,0.,1.));
#6356=DIRECTION('center_axis',(0.,-1.,0.));
#6357=DIRECTION('ref_axis',(1.,0.,0.));
#6358=DIRECTION('',(1.,0.,0.));
#6359=DIRECTION('',(1.,0.,0.));
#6360=DIRECTION('',(0.,0.,1.));
#6361=DIRECTION('center_axis',(-1.,0.,0.));
#6362=DIRECTION('ref_axis',(0.,-1.,0.));
#6363=DIRECTION('',(0.,-1.,0.));
#6364=DIRECTION('',(0.,-1.,0.));
#6365=DIRECTION('center_axis',(0.,0.,1.));
#6366=DIRECTION('ref_axis',(1.,0.,0.));
#6367=DIRECTION('center_axis',(0.,0.,1.));
#6368=DIRECTION('ref_axis',(1.,0.,0.));
#6369=DIRECTION('axis',(0.,0.,1.));
#6370=DIRECTION('refdir',(1.,0.,0.));
#6371=DIRECTION('center_axis',(0.,1.,0.));
#6372=DIRECTION('ref_axis',(-1.,0.,0.));
#6373=DIRECTION('',(-1.,0.,0.));
#6374=DIRECTION('',(0.,0.,1.));
#6375=DIRECTION('',(-1.,0.,0.));
#6376=DIRECTION('',(0.,0.,1.));
#6377=DIRECTION('center_axis',(1.,0.,0.));
#6378=DIRECTION('ref_axis',(0.,1.,0.));
#6379=DIRECTION('',(0.,1.,0.));
#6380=DIRECTION('',(0.,1.,0.));
#6381=DIRECTION('',(0.,0.,1.));
#6382=DIRECTION('center_axis',(0.,-1.,0.));
#6383=DIRECTION('ref_axis',(1.,0.,0.));
#6384=DIRECTION('',(1.,0.,0.));
#6385=DIRECTION('',(1.,0.,0.));
#6386=DIRECTION('',(0.,0.,1.));
#6387=DIRECTION('center_axis',(-1.,0.,0.));
#6388=DIRECTION('ref_axis',(0.,-1.,0.));
#6389=DIRECTION('',(0.,-1.,0.));
#6390=DIRECTION('',(0.,-1.,0.));
#6391=DIRECTION('center_axis',(0.,0.,1.));
#6392=DIRECTION('ref_axis',(1.,0.,0.));
#6393=DIRECTION('center_axis',(0.,0.,1.));
#6394=DIRECTION('ref_axis',(1.,0.,0.));
#6395=DIRECTION('axis',(0.,0.,1.));
#6396=DIRECTION('refdir',(1.,0.,0.));
#6397=DIRECTION('axis',(0.,0.,1.));
#6398=DIRECTION('refdir',(1.,0.,0.));
#6399=DIRECTION('center_axis',(0.,-1.,0.));
#6400=DIRECTION('ref_axis',(0.,0.,-1.));
#6401=DIRECTION('center_axis',(0.,-1.,0.));
#6402=DIRECTION('ref_axis',(1.,0.,0.));
#6403=DIRECTION('center_axis',(0.,-1.,0.));
#6404=DIRECTION('ref_axis',(1.,0.,0.));
#6405=DIRECTION('center_axis',(1.,0.,1.22464679914735E-16));
#6406=DIRECTION('ref_axis',(-1.22464679914735E-16,0.,1.));
#6407=DIRECTION('center_axis',(0.,1.,0.));
#6408=DIRECTION('ref_axis',(1.,0.,0.));
#6409=DIRECTION('center_axis',(0.,1.,0.));
#6410=DIRECTION('ref_axis',(1.,0.,0.));
#6411=DIRECTION('center_axis',(0.,-1.,0.));
#6412=DIRECTION('ref_axis',(1.,0.,0.));
#6413=DIRECTION('',(0.,1.,0.));
#6414=DIRECTION('center_axis',(0.,-1.,0.));
#6415=DIRECTION('ref_axis',(1.,0.,0.));
#6416=DIRECTION('center_axis',(0.,-1.,0.));
#6417=DIRECTION('ref_axis',(1.,0.,0.));
#6418=DIRECTION('center_axis',(0.,-1.,0.));
#6419=DIRECTION('ref_axis',(1.,0.,0.));
#6420=DIRECTION('',(0.,1.,0.));
#6421=DIRECTION('center_axis',(0.,-1.,0.));
#6422=DIRECTION('ref_axis',(1.,0.,0.));
#6423=DIRECTION('center_axis',(0.,1.,0.));
#6424=DIRECTION('ref_axis',(1.,0.,0.));
#6425=DIRECTION('',(-0.707106781186548,0.707106781186547,-8.65956056235494E-17));
#6426=DIRECTION('center_axis',(0.,-1.,0.));
#6427=DIRECTION('ref_axis',(1.,0.,0.));
#6428=DIRECTION('center_axis',(0.,1.,0.));
#6429=DIRECTION('ref_axis',(0.,0.,1.));
#6430=DIRECTION('center_axis',(0.,-1.,0.));
#6431=DIRECTION('ref_axis',(1.,0.,0.));
#6432=DIRECTION('center_axis',(0.,-1.,0.));
#6433=DIRECTION('ref_axis',(1.,0.,0.));
#6434=DIRECTION('',(0.,1.,0.));
#6435=DIRECTION('center_axis',(0.,-1.,0.));
#6436=DIRECTION('ref_axis',(0.,0.,-1.));
#6437=DIRECTION('center_axis',(0.,-1.,0.));
#6438=DIRECTION('ref_axis',(1.,0.,0.));
#6439=DIRECTION('center_axis',(0.,-1.,0.));
#6440=DIRECTION('ref_axis',(1.,0.,0.));
#6441=DIRECTION('',(0.707106781186548,0.707106781186547,8.65956056235494E-17));
#6442=DIRECTION('axis',(0.,0.,1.));
#6443=DIRECTION('refdir',(1.,0.,0.));
#6444=DIRECTION('center_axis',(0.,-1.,0.));
#6445=DIRECTION('ref_axis',(0.,0.,-1.));
#6446=DIRECTION('center_axis',(0.,-1.,0.));
#6447=DIRECTION('ref_axis',(1.,0.,0.));
#6448=DIRECTION('center_axis',(0.,-1.,0.));
#6449=DIRECTION('ref_axis',(1.,0.,0.));
#6450=DIRECTION('center_axis',(1.,0.,1.22464679914735E-16));
#6451=DIRECTION('ref_axis',(-1.22464679914735E-16,0.,1.));
#6452=DIRECTION('center_axis',(0.,1.,0.));
#6453=DIRECTION('ref_axis',(1.,0.,0.));
#6454=DIRECTION('center_axis',(0.,1.,0.));
#6455=DIRECTION('ref_axis',(1.,0.,0.));
#6456=DIRECTION('center_axis',(0.,-1.,0.));
#6457=DIRECTION('ref_axis',(1.,0.,0.));
#6458=DIRECTION('center_axis',(0.,-1.,0.));
#6459=DIRECTION('ref_axis',(1.,0.,0.));
#6460=DIRECTION('',(0.,1.,0.));
#6461=DIRECTION('center_axis',(0.,1.,0.));
#6462=DIRECTION('ref_axis',(0.,0.,1.));
#6463=DIRECTION('center_axis',(0.,-1.,0.));
#6464=DIRECTION('ref_axis',(1.,0.,0.));
#6465=DIRECTION('center_axis',(0.,-1.,0.));
#6466=DIRECTION('ref_axis',(1.,0.,0.));
#6467=DIRECTION('center_axis',(0.,-1.,0.));
#6468=DIRECTION('ref_axis',(1.,0.,0.));
#6469=DIRECTION('center_axis',(0.,-1.,0.));
#6470=DIRECTION('ref_axis',(1.,0.,0.));
#6471=DIRECTION('',(0.707106781186548,0.707106781186547,8.65956056235494E-17));
#6472=DIRECTION('center_axis',(0.,-1.,0.));
#6473=DIRECTION('ref_axis',(1.,0.,0.));
#6474=DIRECTION('center_axis',(0.,-1.,0.));
#6475=DIRECTION('ref_axis',(1.,0.,0.));
#6476=DIRECTION('',(0.,1.,0.));
#6477=DIRECTION('center_axis',(0.,1.,0.));
#6478=DIRECTION('ref_axis',(1.,0.,0.));
#6479=DIRECTION('center_axis',(0.,-1.,0.));
#6480=DIRECTION('ref_axis',(1.,0.,0.));
#6481=DIRECTION('',(-0.707106781186548,0.707106781186547,-8.65956056235494E-17));
#6482=DIRECTION('center_axis',(0.,-1.,0.));
#6483=DIRECTION('ref_axis',(0.,0.,-1.));
#6484=DIRECTION('center_axis',(0.,-1.,0.));
#6485=DIRECTION('ref_axis',(1.,0.,0.));
#6486=DIRECTION('',(0.,1.,0.));
#6487=DIRECTION('axis',(0.,0.,1.));
#6488=DIRECTION('refdir',(1.,0.,0.));
#6489=DIRECTION('center_axis',(0.,0.,1.));
#6490=DIRECTION('ref_axis',(1.,0.,0.));
#6491=DIRECTION('center_axis',(1.22464679914735E-16,-1.,0.));
#6492=DIRECTION('ref_axis',(-1.,-1.22464679914735E-16,0.));
#6493=DIRECTION('center_axis',(0.707106781186548,0.,0.707106781186548));
#6494=DIRECTION('ref_axis',(0.707106781186548,0.,-0.707106781186548));
#6495=DIRECTION('center_axis',(8.65956056235493E-17,-1.,-8.65956056235493E-17));
#6496=DIRECTION('ref_axis',(-0.707106781186548,-1.22464679914735E-16,0.707106781186548));
#6497=DIRECTION('center_axis',(1.,0.,0.));
#6498=DIRECTION('ref_axis',(6.12323399573677E-17,0.,-1.));
#6499=DIRECTION('center_axis',(7.49879891330929E-33,-1.,-1.22464679914735E-16));
#6500=DIRECTION('ref_axis',(-6.12323399573677E-17,-1.22464679914735E-16,
1.));
#6501=DIRECTION('center_axis',(0.707106781186548,0.,-0.707106781186548));
#6502=DIRECTION('ref_axis',(-0.707106781186548,0.,-0.707106781186548));
#6503=DIRECTION('center_axis',(-8.65956056235493E-17,-1.,-8.65956056235493E-17));
#6504=DIRECTION('ref_axis',(0.707106781186548,-1.22464679914735E-16,0.707106781186548));
#6505=DIRECTION('center_axis',(0.,0.,-1.));
#6506=DIRECTION('ref_axis',(-1.,0.,-1.22464679914735E-16));
#6507=DIRECTION('center_axis',(-1.22464679914735E-16,-1.,-1.49975978266186E-32));
#6508=DIRECTION('ref_axis',(1.,-1.22464679914735E-16,1.22464679914735E-16));
#6509=DIRECTION('center_axis',(-0.707106781186548,0.,-0.707106781186548));
#6510=DIRECTION('ref_axis',(-0.707106781186548,0.,0.707106781186548));
#6511=DIRECTION('center_axis',(-8.65956056235493E-17,-1.,8.65956056235493E-17));
#6512=DIRECTION('ref_axis',(0.707106781186548,-1.22464679914735E-16,-0.707106781186548));
#6513=DIRECTION('center_axis',(-1.,0.,0.));
#6514=DIRECTION('ref_axis',(-1.83697019872103E-16,0.,1.));
#6515=DIRECTION('center_axis',(-2.24963967399279E-32,-1.,1.22464679914735E-16));
#6516=DIRECTION('ref_axis',(1.83697019872103E-16,-1.22464679914735E-16,
-1.));
#6517=DIRECTION('center_axis',(-0.707106781186548,0.,0.707106781186548));
#6518=DIRECTION('ref_axis',(0.707106781186548,0.,0.707106781186548));
#6519=DIRECTION('center_axis',(8.65956056235493E-17,-1.,8.65956056235494E-17));
#6520=DIRECTION('ref_axis',(-0.707106781186548,-1.22464679914735E-16,-0.707106781186548));
#6521=DIRECTION('axis',(0.,0.,1.));
#6522=DIRECTION('refdir',(1.,0.,0.));
#6523=DIRECTION('center_axis',(0.,0.,1.));
#6524=DIRECTION('ref_axis',(1.,0.,0.));
#6525=DIRECTION('center_axis',(0.,-1.,0.));
#6526=DIRECTION('ref_axis',(0.,0.,-1.));
#6527=DIRECTION('center_axis',(0.,-1.,0.));
#6528=DIRECTION('ref_axis',(0.,0.,-1.));
#6529=DIRECTION('center_axis',(0.,1.,0.));
#6530=DIRECTION('ref_axis',(1.,0.,0.));
#6531=DIRECTION('center_axis',(0.,1.,0.));
#6532=DIRECTION('ref_axis',(1.,0.,0.));
#6533=DIRECTION('center_axis',(0.,1.,0.));
#6534=DIRECTION('ref_axis',(1.,0.,0.));
#6535=DIRECTION('center_axis',(0.,1.,0.));
#6536=DIRECTION('ref_axis',(1.,0.,0.));
#6537=DIRECTION('',(0.,-1.,0.));
#6538=DIRECTION('center_axis',(0.,-1.,0.));
#6539=DIRECTION('ref_axis',(1.,0.,0.));
#6540=DIRECTION('center_axis',(0.,1.,0.));
#6541=DIRECTION('ref_axis',(1.,0.,0.));
#6542=DIRECTION('center_axis',(0.,1.,0.));
#6543=DIRECTION('ref_axis',(1.,0.,0.));
#6544=DIRECTION('center_axis',(0.,1.,0.));
#6545=DIRECTION('ref_axis',(1.,0.,0.));
#6546=DIRECTION('center_axis',(0.,1.,0.));
#6547=DIRECTION('ref_axis',(1.,0.,0.));
#6548=DIRECTION('center_axis',(0.,1.,0.));
#6549=DIRECTION('ref_axis',(1.,0.,0.));
#6550=DIRECTION('center_axis',(0.,1.,0.));
#6551=DIRECTION('ref_axis',(1.,0.,0.));
#6552=DIRECTION('center_axis',(0.,-1.,0.));
#6553=DIRECTION('ref_axis',(1.,0.,0.));
#6554=DIRECTION('center_axis',(0.,-1.,0.));
#6555=DIRECTION('ref_axis',(0.,0.,-1.));
#6556=DIRECTION('center_axis',(6.12323399573677E-17,0.,1.));
#6557=DIRECTION('ref_axis',(1.,0.,0.));
#6558=DIRECTION('center_axis',(0.,-1.,0.));
#6559=DIRECTION('ref_axis',(0.,0.,-1.));
#6560=DIRECTION('center_axis',(0.,1.,0.));
#6561=DIRECTION('ref_axis',(1.,0.,0.));
#6562=DIRECTION('center_axis',(0.,-1.,0.));
#6563=DIRECTION('ref_axis',(1.,0.,0.));
#6564=DIRECTION('center_axis',(0.,-1.,0.));
#6565=DIRECTION('ref_axis',(0.,0.,-1.));
#6566=DIRECTION('center_axis',(0.,0.,1.));
#6567=DIRECTION('ref_axis',(1.,0.,0.));
#6568=DIRECTION('center_axis',(0.,-1.,0.));
#6569=DIRECTION('ref_axis',(0.,0.,-1.));
#6570=DIRECTION('center_axis',(0.,1.,0.));
#6571=DIRECTION('ref_axis',(1.,0.,0.));
#6572=DIRECTION('center_axis',(0.,-1.,0.));
#6573=DIRECTION('ref_axis',(1.,0.,0.));
#6574=DIRECTION('center_axis',(0.,-1.,0.));
#6575=DIRECTION('ref_axis',(0.,0.,-1.));
#6576=DIRECTION('center_axis',(0.,0.,1.));
#6577=DIRECTION('ref_axis',(1.,0.,0.));
#6578=DIRECTION('center_axis',(0.,-1.,0.));
#6579=DIRECTION('ref_axis',(0.,0.,-1.));
#6580=DIRECTION('center_axis',(0.,1.,0.));
#6581=DIRECTION('ref_axis',(1.,0.,0.));
#6582=DIRECTION('center_axis',(0.,-1.,0.));
#6583=DIRECTION('ref_axis',(1.,0.,0.));
#6584=DIRECTION('center_axis',(0.,-1.,0.));
#6585=DIRECTION('ref_axis',(0.,0.,-1.));
#6586=DIRECTION('center_axis',(0.,0.,1.));
#6587=DIRECTION('ref_axis',(1.,0.,0.));
#6588=DIRECTION('center_axis',(0.,-1.,0.));
#6589=DIRECTION('ref_axis',(0.,0.,-1.));
#6590=DIRECTION('center_axis',(0.,1.,0.));
#6591=DIRECTION('ref_axis',(1.,0.,0.));
#6592=DIRECTION('center_axis',(0.,-1.,0.));
#6593=DIRECTION('ref_axis',(1.,0.,0.));
#6594=DIRECTION('center_axis',(0.,-1.,0.));
#6595=DIRECTION('ref_axis',(0.,0.,-1.));
#6596=DIRECTION('center_axis',(6.12323399573676E-17,0.,1.));
#6597=DIRECTION('ref_axis',(1.,0.,0.));
#6598=DIRECTION('center_axis',(0.,-1.,0.));
#6599=DIRECTION('ref_axis',(0.,0.,-1.));
#6600=DIRECTION('center_axis',(0.,1.,0.));
#6601=DIRECTION('ref_axis',(1.,0.,0.));
#6602=DIRECTION('center_axis',(0.,-1.,0.));
#6603=DIRECTION('ref_axis',(1.,0.,0.));
#6604=DIRECTION('center_axis',(0.,-1.,0.));
#6605=DIRECTION('ref_axis',(0.,0.,-1.));
#6606=DIRECTION('center_axis',(0.,0.,1.));
#6607=DIRECTION('ref_axis',(1.,0.,0.));
#6608=DIRECTION('center_axis',(0.,-1.,0.));
#6609=DIRECTION('ref_axis',(0.,0.,-1.));
#6610=DIRECTION('center_axis',(0.,1.,0.));
#6611=DIRECTION('ref_axis',(1.,0.,0.));
#6612=DIRECTION('center_axis',(0.,1.,0.));
#6613=DIRECTION('ref_axis',(1.,0.,0.));
#6614=DIRECTION('',(0.,1.,0.));
#6615=DIRECTION('center_axis',(0.,-1.,0.));
#6616=DIRECTION('ref_axis',(1.,0.,0.));
#6617=DIRECTION('center_axis',(0.,-1.,0.));
#6618=DIRECTION('ref_axis',(1.,0.,0.));
#6619=DIRECTION('center_axis',(0.,1.,0.));
#6620=DIRECTION('ref_axis',(1.,0.,0.));
#6621=DIRECTION('center_axis',(0.,-1.,0.));
#6622=DIRECTION('ref_axis',(0.,0.,-1.));
#6623=DIRECTION('center_axis',(0.,0.,1.));
#6624=DIRECTION('ref_axis',(1.,0.,0.));
#6625=DIRECTION('center_axis',(0.,-1.,0.));
#6626=DIRECTION('ref_axis',(0.,0.,-1.));
#6627=DIRECTION('center_axis',(0.,-1.,0.));
#6628=DIRECTION('ref_axis',(-1.,0.,0.));
#6629=DIRECTION('center_axis',(0.,1.,0.));
#6630=DIRECTION('ref_axis',(1.,0.,0.));
#6631=DIRECTION('axis',(0.,0.,1.));
#6632=DIRECTION('refdir',(1.,0.,0.));
#6633=DIRECTION('center_axis',(0.,1.,0.));
#6634=DIRECTION('ref_axis',(0.,0.,1.));
#6635=DIRECTION('center_axis',(0.,-1.,0.));
#6636=DIRECTION('ref_axis',(1.,0.,0.));
#6637=DIRECTION('center_axis',(0.,-1.,0.));
#6638=DIRECTION('ref_axis',(1.,0.,0.));
#6639=DIRECTION('center_axis',(0.,-1.,0.));
#6640=DIRECTION('ref_axis',(1.,0.,0.));
#6641=DIRECTION('center_axis',(0.,-1.,0.));
#6642=DIRECTION('ref_axis',(1.,0.,0.));
#6643=DIRECTION('',(0.,1.,0.));
#6644=DIRECTION('center_axis',(0.,-1.,0.));
#6645=DIRECTION('ref_axis',(0.,0.,-1.));
#6646=DIRECTION('center_axis',(0.,-1.,0.));
#6647=DIRECTION('ref_axis',(1.,0.,0.));
#6648=DIRECTION('center_axis',(0.,-1.,0.));
#6649=DIRECTION('ref_axis',(1.,0.,0.));
#6650=DIRECTION('',(0.,1.,0.));
#6651=DIRECTION('center_axis',(0.,1.,0.));
#6652=DIRECTION('ref_axis',(0.,0.,1.));
#6653=DIRECTION('center_axis',(0.,-1.,0.));
#6654=DIRECTION('ref_axis',(1.,0.,0.));
#6655=DIRECTION('center_axis',(0.,-1.,0.));
#6656=DIRECTION('ref_axis',(1.,0.,0.));
#6657=DIRECTION('center_axis',(0.,-1.,0.));
#6658=DIRECTION('ref_axis',(1.,0.,0.));
#6659=DIRECTION('center_axis',(0.,-1.,0.));
#6660=DIRECTION('ref_axis',(1.,0.,0.));
#6661=DIRECTION('',(0.,1.,0.));
#6662=DIRECTION('center_axis',(0.,-1.,0.));
#6663=DIRECTION('ref_axis',(0.,0.,-1.));
#6664=DIRECTION('center_axis',(0.,-1.,0.));
#6665=DIRECTION('ref_axis',(1.,0.,0.));
#6666=DIRECTION('center_axis',(0.,-1.,0.));
#6667=DIRECTION('ref_axis',(1.,0.,0.));
#6668=DIRECTION('',(0.,1.,0.));
#6669=DIRECTION('',(0.,0.,1.));
#6670=DIRECTION('',(1.,0.,0.));
#6671=DIRECTION('',(0.,0.,1.));
#6672=DIRECTION('',(1.,0.,0.));
#6673=DIRECTION('',(0.,0.,1.));
#6674=DIRECTION('',(1.,0.,0.));
#6675=DIRECTION('',(0.,0.,1.));
#6676=DIRECTION('',(1.,0.,0.));
#6677=DIRECTION('',(0.,0.,1.));
#6678=DIRECTION('',(1.,0.,0.));
#6679=DIRECTION('axis',(0.,0.,1.));
#6680=DIRECTION('refdir',(1.,0.,0.));
#6681=DIRECTION('center_axis',(0.,1.,0.));
#6682=DIRECTION('ref_axis',(0.,0.,1.));
#6683=DIRECTION('center_axis',(0.,-1.,0.));
#6684=DIRECTION('ref_axis',(1.,0.,0.));
#6685=DIRECTION('center_axis',(0.,-1.,0.));
#6686=DIRECTION('ref_axis',(1.,0.,0.));
#6687=DIRECTION('center_axis',(0.,-1.,0.));
#6688=DIRECTION('ref_axis',(1.,0.,0.));
#6689=DIRECTION('',(0.707106781186548,0.707106781186547,8.65956056235494E-17));
#6690=DIRECTION('center_axis',(0.,-1.,0.));
#6691=DIRECTION('ref_axis',(1.,0.,0.));
#6692=DIRECTION('center_axis',(0.,-1.,0.));
#6693=DIRECTION('ref_axis',(1.,0.,0.));
#6694=DIRECTION('',(0.,1.,0.));
#6695=DIRECTION('center_axis',(0.,1.,0.));
#6696=DIRECTION('ref_axis',(1.,0.,0.));
#6697=DIRECTION('center_axis',(0.,-1.,0.));
#6698=DIRECTION('ref_axis',(1.,0.,0.));
#6699=DIRECTION('',(-0.707106781186547,0.707106781186548,-8.65956056235493E-17));
#6700=DIRECTION('center_axis',(0.,-1.,0.));
#6701=DIRECTION('ref_axis',(0.,0.,-1.));
#6702=DIRECTION('center_axis',(0.,-1.,0.));
#6703=DIRECTION('ref_axis',(1.,0.,0.));
#6704=DIRECTION('center_axis',(0.,1.,0.));
#6705=DIRECTION('ref_axis',(1.,0.,0.));
#6706=DIRECTION('center_axis',(0.,1.,0.));
#6707=DIRECTION('ref_axis',(1.,0.,0.));
#6708=DIRECTION('',(-0.447213595499958,0.894427190999916,-5.47678698264203E-17));
#6709=DIRECTION('center_axis',(0.,-1.,0.));
#6710=DIRECTION('ref_axis',(1.,0.,0.));
#6711=DIRECTION('center_axis',(0.,1.,0.));
#6712=DIRECTION('ref_axis',(1.,0.,0.));
#6713=DIRECTION('',(0.,1.,0.));
#6714=DIRECTION('center_axis',(0.,1.,0.));
#6715=DIRECTION('ref_axis',(1.,0.,0.));
#6716=DIRECTION('center_axis',(0.,-1.,0.));
#6717=DIRECTION('ref_axis',(1.,0.,0.));
#6718=DIRECTION('',(-0.707106781186547,0.707106781186548,-8.65956056235493E-17));
#6719=DIRECTION('center_axis',(0.,-1.,0.));
#6720=DIRECTION('ref_axis',(0.,0.,-1.));
#6721=DIRECTION('center_axis',(0.866025403784439,0.,-0.5));
#6722=DIRECTION('ref_axis',(0.5,0.,0.866025403784439));
#6723=DIRECTION('',(-0.5,0.,-0.866025403784439));
#6724=DIRECTION('',(0.,-1.,0.));
#6725=DIRECTION('',(0.5,0.,0.866025403784439));
#6726=DIRECTION('',(0.,-1.,0.));
#6727=DIRECTION('center_axis',(1.92296268638356E-16,0.,-1.));
#6728=DIRECTION('ref_axis',(1.,0.,1.92296268638356E-16));
#6729=DIRECTION('',(-1.,0.,-1.92296268638356E-16));
#6730=DIRECTION('',(0.,-1.,0.));
#6731=DIRECTION('',(1.,0.,1.92296268638356E-16));
#6732=DIRECTION('center_axis',(-0.866025403784439,0.,-0.5));
#6733=DIRECTION('ref_axis',(0.5,0.,-0.866025403784439));
#6734=DIRECTION('',(-0.5,0.,0.866025403784438));
#6735=DIRECTION('',(0.,-1.,0.));
#6736=DIRECTION('',(0.5,0.,-0.866025403784438));
#6737=DIRECTION('center_axis',(-0.866025403784439,0.,0.5));
#6738=DIRECTION('ref_axis',(-0.5,0.,-0.866025403784439));
#6739=DIRECTION('',(0.5,0.,0.866025403784439));
#6740=DIRECTION('',(0.,-1.,0.));
#6741=DIRECTION('',(-0.5,0.,-0.866025403784439));
#6742=DIRECTION('center_axis',(-1.92296268638356E-16,0.,1.));
#6743=DIRECTION('ref_axis',(-1.,0.,-1.92296268638356E-16));
#6744=DIRECTION('',(1.,0.,1.92296268638356E-16));
#6745=DIRECTION('',(0.,-1.,0.));
#6746=DIRECTION('',(-1.,0.,-1.92296268638356E-16));
#6747=DIRECTION('center_axis',(0.866025403784439,0.,0.5));
#6748=DIRECTION('ref_axis',(-0.5,0.,0.866025403784439));
#6749=DIRECTION('',(0.5,0.,-0.866025403784439));
#6750=DIRECTION('',(-0.5,0.,0.866025403784439));
#6751=DIRECTION('center_axis',(0.,1.,0.));
#6752=DIRECTION('ref_axis',(1.,0.,0.));
#6753=DIRECTION('center_axis',(0.,-1.,0.));
#6754=DIRECTION('ref_axis',(0.,0.,-1.));
#6755=DIRECTION('axis',(0.,0.,1.));
#6756=DIRECTION('refdir',(1.,0.,0.));
#6757=DIRECTION('center_axis',(0.,1.,0.));
#6758=DIRECTION('ref_axis',(0.,0.,1.));
#6759=DIRECTION('center_axis',(0.,-1.,0.));
#6760=DIRECTION('ref_axis',(1.,0.,0.));
#6761=DIRECTION('center_axis',(0.,-1.,0.));
#6762=DIRECTION('ref_axis',(1.,0.,0.));
#6763=DIRECTION('center_axis',(0.,-1.,0.));
#6764=DIRECTION('ref_axis',(1.,0.,0.));
#6765=DIRECTION('',(0.707106781186547,0.707106781186548,8.65956056235493E-17));
#6766=DIRECTION('center_axis',(0.,-1.,0.));
#6767=DIRECTION('ref_axis',(1.,0.,0.));
#6768=DIRECTION('center_axis',(0.,-1.,0.));
#6769=DIRECTION('ref_axis',(1.,0.,0.));
#6770=DIRECTION('',(0.,1.,0.));
#6771=DIRECTION('center_axis',(0.,1.,0.));
#6772=DIRECTION('ref_axis',(1.,0.,0.));
#6773=DIRECTION('center_axis',(0.,-1.,0.));
#6774=DIRECTION('ref_axis',(1.,0.,0.));
#6775=DIRECTION('',(-0.707106781186547,0.707106781186548,-8.65956056235493E-17));
#6776=DIRECTION('center_axis',(0.,-1.,0.));
#6777=DIRECTION('ref_axis',(0.,0.,-1.));
#6778=DIRECTION('center_axis',(0.,-1.,0.));
#6779=DIRECTION('ref_axis',(1.,0.,0.));
#6780=DIRECTION('center_axis',(0.,1.,0.));
#6781=DIRECTION('ref_axis',(1.,0.,0.));
#6782=DIRECTION('center_axis',(0.,1.,0.));
#6783=DIRECTION('ref_axis',(1.,0.,0.));
#6784=DIRECTION('',(-0.447213595499958,0.894427190999916,-5.47678698264203E-17));
#6785=DIRECTION('center_axis',(0.,-1.,0.));
#6786=DIRECTION('ref_axis',(1.,0.,0.));
#6787=DIRECTION('center_axis',(0.,1.,0.));
#6788=DIRECTION('ref_axis',(1.,0.,0.));
#6789=DIRECTION('',(0.,1.,0.));
#6790=DIRECTION('center_axis',(0.,1.,0.));
#6791=DIRECTION('ref_axis',(1.,0.,0.));
#6792=DIRECTION('center_axis',(0.,-1.,0.));
#6793=DIRECTION('ref_axis',(1.,0.,0.));
#6794=DIRECTION('',(-0.707106781186547,0.707106781186548,-8.65956056235493E-17));
#6795=DIRECTION('center_axis',(0.,-1.,0.));
#6796=DIRECTION('ref_axis',(0.,0.,-1.));
#6797=DIRECTION('center_axis',(0.866025403784439,0.,-0.5));
#6798=DIRECTION('ref_axis',(0.5,0.,0.866025403784439));
#6799=DIRECTION('',(-0.5,0.,-0.866025403784439));
#6800=DIRECTION('',(0.,-1.,0.));
#6801=DIRECTION('',(0.5,0.,0.866025403784439));
#6802=DIRECTION('',(0.,-1.,0.));
#6803=DIRECTION('center_axis',(1.60246890531964E-16,0.,-1.));
#6804=DIRECTION('ref_axis',(1.,0.,1.60246890531964E-16));
#6805=DIRECTION('',(-1.,0.,-1.60246890531964E-16));
#6806=DIRECTION('',(0.,-1.,0.));
#6807=DIRECTION('',(1.,0.,1.60246890531964E-16));
#6808=DIRECTION('center_axis',(-0.866025403784439,0.,-0.5));
#6809=DIRECTION('ref_axis',(0.5,0.,-0.866025403784439));
#6810=DIRECTION('',(-0.5,0.,0.866025403784439));
#6811=DIRECTION('',(0.,-1.,0.));
#6812=DIRECTION('',(0.5,0.,-0.866025403784439));
#6813=DIRECTION('center_axis',(-0.866025403784439,0.,0.5));
#6814=DIRECTION('ref_axis',(-0.5,0.,-0.866025403784439));
#6815=DIRECTION('',(0.5,0.,0.866025403784439));
#6816=DIRECTION('',(0.,-1.,0.));
#6817=DIRECTION('',(-0.5,0.,-0.866025403784439));
#6818=DIRECTION('center_axis',(-1.60246890531964E-16,0.,1.));
#6819=DIRECTION('ref_axis',(-1.,0.,-1.60246890531964E-16));
#6820=DIRECTION('',(1.,0.,1.60246890531964E-16));
#6821=DIRECTION('',(0.,-1.,0.));
#6822=DIRECTION('',(-1.,0.,-1.60246890531964E-16));
#6823=DIRECTION('center_axis',(0.866025403784439,0.,0.5));
#6824=DIRECTION('ref_axis',(-0.5,0.,0.866025403784439));
#6825=DIRECTION('',(0.5,0.,-0.866025403784439));
#6826=DIRECTION('',(-0.5,0.,0.866025403784439));
#6827=DIRECTION('center_axis',(0.,1.,0.));
#6828=DIRECTION('ref_axis',(1.,0.,0.));
#6829=DIRECTION('center_axis',(0.,-1.,0.));
#6830=DIRECTION('ref_axis',(0.,0.,-1.));
#6831=DIRECTION('axis',(0.,0.,1.));
#6832=DIRECTION('refdir',(1.,0.,0.));
#6833=DIRECTION('axis',(0.,0.,1.));
#6834=DIRECTION('refdir',(1.,0.,0.));
#6835=DIRECTION('center_axis',(0.,1.,0.));
#6836=DIRECTION('ref_axis',(1.,0.,0.));
#6837=DIRECTION('center_axis',(0.,1.,0.));
#6838=DIRECTION('ref_axis',(1.,0.,0.));
#6839=DIRECTION('',(0.,1.,0.));
#6840=DIRECTION('center_axis',(0.,-1.,0.));
#6841=DIRECTION('ref_axis',(1.,0.,0.));
#6842=DIRECTION('center_axis',(0.,1.,0.));
#6843=DIRECTION('ref_axis',(1.,0.,0.));
#6844=DIRECTION('center_axis',(-1.,0.,0.));
#6845=DIRECTION('ref_axis',(0.,0.,1.));
#6846=DIRECTION('',(0.,-1.,0.));
#6847=DIRECTION('',(0.,0.,-1.));
#6848=DIRECTION('',(0.,1.,0.));
#6849=DIRECTION('',(0.,0.,-1.));
#6850=DIRECTION('center_axis',(0.,1.,0.));
#6851=DIRECTION('ref_axis',(1.,0.,0.));
#6852=DIRECTION('center_axis',(0.,-1.,0.));
#6853=DIRECTION('ref_axis',(1.,0.,0.));
#6854=DIRECTION('',(-1.,0.,0.));
#6855=DIRECTION('',(0.,0.,1.));
#6856=DIRECTION('center_axis',(1.,0.,0.));
#6857=DIRECTION('ref_axis',(0.,0.,-1.));
#6858=DIRECTION('',(0.,1.,0.));
#6859=DIRECTION('',(0.,1.,0.));
#6860=DIRECTION('',(0.,0.,1.));
#6861=DIRECTION('center_axis',(0.,0.,1.));
#6862=DIRECTION('ref_axis',(1.,0.,0.));
#6863=DIRECTION('',(-1.,0.,0.));
#6864=DIRECTION('center_axis',(0.,1.,0.));
#6865=DIRECTION('ref_axis',(1.,0.,0.));
#6866=DIRECTION('center_axis',(0.,1.,0.));
#6867=DIRECTION('ref_axis',(1.,0.,0.));
#6868=DIRECTION('',(0.,-1.,0.));
#6869=DIRECTION('center_axis',(0.,1.,0.));
#6870=DIRECTION('ref_axis',(1.,0.,0.));
#6871=DIRECTION('center_axis',(0.,1.,0.));
#6872=DIRECTION('ref_axis',(1.,0.,0.));
#6873=DIRECTION('center_axis',(0.,1.,0.));
#6874=DIRECTION('ref_axis',(1.,0.,0.));
#6875=DIRECTION('center_axis',(0.,1.,0.));
#6876=DIRECTION('ref_axis',(1.,0.,0.));
#6877=DIRECTION('center_axis',(0.,1.,0.));
#6878=DIRECTION('ref_axis',(1.,0.,0.));
#6879=DIRECTION('center_axis',(0.,-1.,0.));
#6880=DIRECTION('ref_axis',(1.,0.,0.));
#6881=DIRECTION('center_axis',(0.,1.,0.));
#6882=DIRECTION('ref_axis',(1.,0.,0.));
#6883=DIRECTION('center_axis',(0.,1.,0.));
#6884=DIRECTION('ref_axis',(1.,0.,0.));
#6885=DIRECTION('center_axis',(0.,-1.,0.));
#6886=DIRECTION('ref_axis',(1.,0.,0.));
#6887=DIRECTION('center_axis',(0.,1.,0.));
#6888=DIRECTION('ref_axis',(1.,0.,0.));
#6889=DIRECTION('center_axis',(0.,1.,0.));
#6890=DIRECTION('ref_axis',(1.,0.,0.));
#6891=DIRECTION('center_axis',(0.,1.,0.));
#6892=DIRECTION('ref_axis',(1.,0.,0.));
#6893=DIRECTION('',(0.,-1.,0.));
#6894=DIRECTION('center_axis',(0.,1.,0.));
#6895=DIRECTION('ref_axis',(1.,0.,0.));
#6896=DIRECTION('center_axis',(0.,-1.,0.));
#6897=DIRECTION('ref_axis',(1.,0.,0.));
#6898=DIRECTION('',(0.,1.,0.));
#6899=DIRECTION('center_axis',(0.,1.,0.));
#6900=DIRECTION('ref_axis',(1.,0.,0.));
#6901=DIRECTION('',(0.,-1.,0.));
#6902=DIRECTION('center_axis',(0.,1.,0.));
#6903=DIRECTION('ref_axis',(1.,0.,0.));
#6904=DIRECTION('center_axis',(0.,1.,0.));
#6905=DIRECTION('ref_axis',(1.,0.,0.));
#6906=DIRECTION('center_axis',(0.,1.,0.));
#6907=DIRECTION('ref_axis',(1.,0.,0.));
#6908=DIRECTION('',(0.,1.,0.));
#6909=DIRECTION('center_axis',(0.,1.,0.));
#6910=DIRECTION('ref_axis',(1.,0.,0.));
#6911=DIRECTION('center_axis',(0.,1.,0.));
#6912=DIRECTION('ref_axis',(1.,0.,0.));
#6913=DIRECTION('center_axis',(1.,0.,0.));
#6914=DIRECTION('ref_axis',(0.,0.,-1.));
#6915=DIRECTION('',(1.,0.,0.));
#6916=DIRECTION('center_axis',(0.,1.,0.));
#6917=DIRECTION('ref_axis',(1.,0.,0.));
#6918=DIRECTION('',(0.,1.,0.));
#6919=DIRECTION('center_axis',(0.,1.,0.));
#6920=DIRECTION('ref_axis',(1.,0.,0.));
#6921=DIRECTION('center_axis',(0.,1.,0.));
#6922=DIRECTION('ref_axis',(1.,0.,0.));
#6923=DIRECTION('center_axis',(0.,1.,0.));
#6924=DIRECTION('ref_axis',(1.,0.,0.));
#6925=DIRECTION('center_axis',(0.,1.,0.));
#6926=DIRECTION('ref_axis',(1.,0.,0.));
#6927=DIRECTION('axis',(0.,0.,1.));
#6928=DIRECTION('refdir',(1.,0.,0.));
#6929=DIRECTION('center_axis',(0.,1.,0.));
#6930=DIRECTION('ref_axis',(1.,0.,0.));
#6931=DIRECTION('center_axis',(0.,-1.,0.));
#6932=DIRECTION('ref_axis',(1.,0.,0.));
#6933=DIRECTION('',(0.,-1.,0.));
#6934=DIRECTION('center_axis',(0.,-1.,0.));
#6935=DIRECTION('ref_axis',(1.,0.,0.));
#6936=DIRECTION('center_axis',(0.,1.,0.));
#6937=DIRECTION('ref_axis',(1.,0.,0.));
#6938=DIRECTION('center_axis',(0.,1.,0.));
#6939=DIRECTION('ref_axis',(1.,0.,0.));
#6940=DIRECTION('',(0.,-1.,0.));
#6941=DIRECTION('center_axis',(0.,1.,0.));
#6942=DIRECTION('ref_axis',(1.,0.,0.));
#6943=DIRECTION('center_axis',(0.,1.,0.));
#6944=DIRECTION('ref_axis',(1.,0.,0.));
#6945=DIRECTION('center_axis',(0.,1.,0.));
#6946=DIRECTION('ref_axis',(1.,0.,0.));
#6947=DIRECTION('axis',(0.,0.,1.));
#6948=DIRECTION('refdir',(1.,0.,0.));
#6949=DIRECTION('center_axis',(0.,0.,1.));
#6950=DIRECTION('ref_axis',(1.,0.,0.));
#6951=DIRECTION('',(0.,1.,0.));
#6952=DIRECTION('center_axis',(0.,0.,1.));
#6953=DIRECTION('ref_axis',(1.,0.,0.));
#6954=DIRECTION('center_axis',(0.,0.,1.));
#6955=DIRECTION('ref_axis',(1.,0.,0.));
#6956=DIRECTION('center_axis',(0.,0.,1.));
#6957=DIRECTION('ref_axis',(1.,0.,0.));
#6958=DIRECTION('',(0.,0.,1.));
#6959=DIRECTION('center_axis',(0.,0.,1.));
#6960=DIRECTION('ref_axis',(1.,0.,0.));
#6961=DIRECTION('center_axis',(0.,0.,1.));
#6962=DIRECTION('ref_axis',(1.,0.,0.));
#6963=DIRECTION('',(0.,-1.,0.));
#6964=DIRECTION('center_axis',(0.,1.,0.));
#6965=DIRECTION('ref_axis',(1.,0.,0.));
#6966=DIRECTION('center_axis',(0.,-1.,0.));
#6967=DIRECTION('ref_axis',(1.,0.,0.));
#6968=DIRECTION('',(0.,-1.,0.));
#6969=DIRECTION('center_axis',(0.,-1.,0.));
#6970=DIRECTION('ref_axis',(1.,0.,0.));
#6971=DIRECTION('center_axis',(0.,1.,0.));
#6972=DIRECTION('ref_axis',(1.,0.,0.));
#6973=DIRECTION('center_axis',(0.,1.,0.));
#6974=DIRECTION('ref_axis',(1.,0.,0.));
#6975=DIRECTION('',(0.,-1.,0.));
#6976=DIRECTION('center_axis',(0.,1.,0.));
#6977=DIRECTION('ref_axis',(1.,0.,0.));
#6978=DIRECTION('center_axis',(0.,1.,0.));
#6979=DIRECTION('ref_axis',(1.,0.,0.));
#6980=DIRECTION('center_axis',(0.,1.,0.));
#6981=DIRECTION('ref_axis',(1.,0.,0.));
#6982=DIRECTION('axis',(0.,0.,1.));
#6983=DIRECTION('refdir',(1.,0.,0.));
#6984=DIRECTION('center_axis',(-1.,0.,0.));
#6985=DIRECTION('ref_axis',(0.,0.,1.));
#6986=DIRECTION('',(0.,0.,1.));
#6987=DIRECTION('',(0.,1.,0.));
#6988=DIRECTION('',(0.,0.,-1.));
#6989=DIRECTION('',(0.,1.,0.));
#6990=DIRECTION('center_axis',(0.,0.,-1.));
#6991=DIRECTION('ref_axis',(-1.,0.,0.));
#6992=DIRECTION('',(-1.,0.,0.));
#6993=DIRECTION('',(0.,1.,0.));
#6994=DIRECTION('',(1.,0.,0.));
#6995=DIRECTION('center_axis',(1.,0.,0.));
#6996=DIRECTION('ref_axis',(0.,0.,-1.));
#6997=DIRECTION('',(0.,0.,-1.));
#6998=DIRECTION('',(0.,-1.,0.));
#6999=DIRECTION('',(0.,0.,1.));
#7000=DIRECTION('center_axis',(0.,1.,0.));
#7001=DIRECTION('ref_axis',(1.,0.,0.));
#7002=DIRECTION('center_axis',(0.,1.,0.));
#7003=DIRECTION('ref_axis',(1.,0.,0.));
#7004=DIRECTION('center_axis',(0.,-1.,0.));
#7005=DIRECTION('ref_axis',(1.,0.,0.));
#7006=DIRECTION('center_axis',(0.,-1.,0.));
#7007=DIRECTION('ref_axis',(1.,0.,0.));
#7008=DIRECTION('center_axis',(0.,-1.,0.));
#7009=DIRECTION('ref_axis',(1.,0.,0.));
#7010=DIRECTION('center_axis',(0.,-1.,0.));
#7011=DIRECTION('ref_axis',(1.,0.,0.));
#7012=DIRECTION('center_axis',(0.,-1.,0.));
#7013=DIRECTION('ref_axis',(1.,0.,0.));
#7014=DIRECTION('center_axis',(0.,1.,0.));
#7015=DIRECTION('ref_axis',(-1.83697019872103E-16,0.,1.));
#7016=DIRECTION('center_axis',(0.,-1.,0.));
#7017=DIRECTION('ref_axis',(1.,0.,0.));
#7018=DIRECTION('center_axis',(0.,1.,0.));
#7019=DIRECTION('ref_axis',(1.,0.,0.));
#7020=DIRECTION('center_axis',(0.,1.,0.));
#7021=DIRECTION('ref_axis',(1.,0.,0.));
#7022=DIRECTION('',(0.,1.,0.));
#7023=DIRECTION('center_axis',(0.,1.,0.));
#7024=DIRECTION('ref_axis',(1.,0.,0.));
#7025=DIRECTION('center_axis',(0.,1.,0.));
#7026=DIRECTION('ref_axis',(1.,0.,0.));
#7027=DIRECTION('',(0.,1.,0.));
#7028=DIRECTION('center_axis',(0.,1.,0.));
#7029=DIRECTION('ref_axis',(1.,0.,0.));
#7030=DIRECTION('center_axis',(0.,1.,0.));
#7031=DIRECTION('ref_axis',(1.,0.,0.));
#7032=DIRECTION('',(0.,1.,0.));
#7033=DIRECTION('center_axis',(0.,1.,0.));
#7034=DIRECTION('ref_axis',(1.,0.,0.));
#7035=DIRECTION('center_axis',(0.,1.,0.));
#7036=DIRECTION('ref_axis',(1.,0.,0.));
#7037=DIRECTION('',(0.,1.,0.));
#7038=DIRECTION('center_axis',(0.,1.,0.));
#7039=DIRECTION('ref_axis',(1.,0.,0.));
#7040=DIRECTION('center_axis',(0.,1.,0.));
#7041=DIRECTION('ref_axis',(1.,0.,0.));
#7042=DIRECTION('center_axis',(0.,-1.,0.));
#7043=DIRECTION('ref_axis',(1.,0.,0.));
#7044=DIRECTION('center_axis',(0.,1.,0.));
#7045=DIRECTION('ref_axis',(1.,0.,0.));
#7046=DIRECTION('',(0.,-1.,0.));
#7047=DIRECTION('center_axis',(0.,1.,0.));
#7048=DIRECTION('ref_axis',(1.,0.,0.));
#7049=DIRECTION('',(0.,-1.,0.));
#7050=DIRECTION('center_axis',(0.,1.,0.));
#7051=DIRECTION('ref_axis',(1.,0.,0.));
#7052=DIRECTION('center_axis',(0.,1.,0.));
#7053=DIRECTION('ref_axis',(1.,0.,0.));
#7054=DIRECTION('axis',(0.,0.,1.));
#7055=DIRECTION('refdir',(1.,0.,0.));
#7056=DIRECTION('center_axis',(0.,1.,0.));
#7057=DIRECTION('ref_axis',(1.,0.,0.));
#7058=DIRECTION('center_axis',(0.,-1.,0.));
#7059=DIRECTION('ref_axis',(1.,0.,0.));
#7060=DIRECTION('',(0.,-1.,0.));
#7061=DIRECTION('center_axis',(0.,-1.,0.));
#7062=DIRECTION('ref_axis',(1.,0.,0.));
#7063=DIRECTION('center_axis',(0.,1.,0.));
#7064=DIRECTION('ref_axis',(1.,0.,0.));
#7065=DIRECTION('center_axis',(0.,1.,0.));
#7066=DIRECTION('ref_axis',(1.,0.,0.));
#7067=DIRECTION('',(0.,-1.,0.));
#7068=DIRECTION('center_axis',(0.,1.,0.));
#7069=DIRECTION('ref_axis',(1.,0.,0.));
#7070=DIRECTION('center_axis',(0.,1.,0.));
#7071=DIRECTION('ref_axis',(1.,0.,0.));
#7072=DIRECTION('center_axis',(0.,1.,0.));
#7073=DIRECTION('ref_axis',(1.,0.,0.));
#7074=DIRECTION('axis',(0.,0.,1.));
#7075=DIRECTION('refdir',(1.,0.,0.));
#7076=DIRECTION('center_axis',(0.,1.,0.));
#7077=DIRECTION('ref_axis',(1.,0.,0.));
#7078=DIRECTION('',(-0.5,0.,0.866025403784439));
#7079=DIRECTION('',(-1.,0.,-3.29650746237182E-16));
#7080=DIRECTION('',(-0.5,0.,-0.866025403784439));
#7081=DIRECTION('',(0.5,0.,-0.866025403784438));
#7082=DIRECTION('',(1.,0.,0.));
#7083=DIRECTION('',(0.5,0.,0.866025403784439));
#7084=DIRECTION('center_axis',(0.,-1.,0.));
#7085=DIRECTION('ref_axis',(1.,0.,0.));
#7086=DIRECTION('center_axis',(0.,1.,0.));
#7087=DIRECTION('ref_axis',(1.,0.,0.));
#7088=DIRECTION('',(0.5,0.,-0.866025403784439));
#7089=DIRECTION('',(-0.5,0.,-0.866025403784439));
#7090=DIRECTION('',(-1.,0.,0.));
#7091=DIRECTION('',(-0.5,0.,0.866025403784438));
#7092=DIRECTION('',(0.5,0.,0.866025403784439));
#7093=DIRECTION('',(1.,0.,3.29650746237182E-16));
#7094=DIRECTION('center_axis',(0.,1.,0.));
#7095=DIRECTION('ref_axis',(1.,0.,0.));
#7096=DIRECTION('center_axis',(-3.29650746237182E-16,0.,1.));
#7097=DIRECTION('ref_axis',(1.,0.,3.29650746237182E-16));
#7098=DIRECTION('',(0.,-1.,0.));
#7099=DIRECTION('',(0.,1.,0.));
#7100=DIRECTION('center_axis',(-0.866025403784439,0.,0.5));
#7101=DIRECTION('ref_axis',(0.5,0.,0.866025403784439));
#7102=DIRECTION('',(0.,1.,0.));
#7103=DIRECTION('center_axis',(-0.866025403784439,0.,-0.5));
#7104=DIRECTION('ref_axis',(-0.5,0.,0.866025403784439));
#7105=DIRECTION('',(0.,1.,0.));
#7106=DIRECTION('center_axis',(0.,0.,-1.));
#7107=DIRECTION('ref_axis',(-1.,0.,0.));
#7108=DIRECTION('',(0.,1.,0.));
#7109=DIRECTION('center_axis',(0.866025403784439,0.,-0.5));
#7110=DIRECTION('ref_axis',(-0.5,0.,-0.866025403784439));
#7111=DIRECTION('',(0.,1.,0.));
#7112=DIRECTION('center_axis',(0.866025403784439,0.,0.5));
#7113=DIRECTION('ref_axis',(0.5,0.,-0.866025403784439));
#7114=DIRECTION('center_axis',(0.,-1.,0.));
#7115=DIRECTION('ref_axis',(1.,0.,0.));
#7116=DIRECTION('',(0.,1.,0.));
#7117=DIRECTION('center_axis',(0.,-1.,0.));
#7118=DIRECTION('ref_axis',(1.,0.,0.));
#7119=DIRECTION('center_axis',(0.,1.,0.));
#7120=DIRECTION('ref_axis',(0.,0.,1.));
#7121=DIRECTION('center_axis',(0.,-1.,0.));
#7122=DIRECTION('ref_axis',(1.,0.,0.));
#7123=DIRECTION('center_axis',(0.,-1.,0.));
#7124=DIRECTION('ref_axis',(1.,0.,0.));
#7125=DIRECTION('center_axis',(0.,-1.,0.));
#7126=DIRECTION('ref_axis',(1.,0.,0.));
#7127=DIRECTION('',(0.707106781186547,0.707106781186548,8.65956056235493E-17));
#7128=DIRECTION('center_axis',(0.,-1.,0.));
#7129=DIRECTION('ref_axis',(1.,0.,0.));
#7130=DIRECTION('center_axis',(0.,-1.,0.));
#7131=DIRECTION('ref_axis',(1.,0.,0.));
#7132=DIRECTION('',(0.,1.,0.));
#7133=DIRECTION('center_axis',(0.,1.,0.));
#7134=DIRECTION('ref_axis',(1.,0.,0.));
#7135=DIRECTION('center_axis',(0.,-1.,0.));
#7136=DIRECTION('ref_axis',(1.,0.,0.));
#7137=DIRECTION('',(-0.707106781186547,0.707106781186548,-8.65956056235493E-17));
#7138=DIRECTION('center_axis',(0.,-1.,0.));
#7139=DIRECTION('ref_axis',(0.,0.,-1.));
#7140=DIRECTION('center_axis',(0.,-1.,0.));
#7141=DIRECTION('ref_axis',(1.,0.,0.));
#7142=DIRECTION('center_axis',(0.,-1.,0.));
#7143=DIRECTION('ref_axis',(1.,0.,0.));
#7144=DIRECTION('',(0.,1.,0.));
#7145=DIRECTION('',(0.,0.,1.));
#7146=DIRECTION('',(1.,0.,0.));
#7147=DIRECTION('',(0.,0.,1.));
#7148=DIRECTION('',(1.,0.,0.));
#7149=DIRECTION('',(0.,0.,1.));
#7150=DIRECTION('',(1.,0.,0.));
#7151=DIRECTION('',(0.,0.,1.));
#7152=DIRECTION('',(1.,0.,0.));
#7153=DIRECTION('',(0.,0.,1.));
#7154=DIRECTION('',(1.,0.,0.));
#7155=DIRECTION('',(0.,0.,1.));
#7156=DIRECTION('',(1.,0.,0.));
#7157=DIRECTION('',(0.,0.,1.));
#7158=DIRECTION('',(1.,0.,0.));
#7159=DIRECTION('',(0.,0.,1.));
#7160=DIRECTION('',(1.,0.,0.));
#7161=DIRECTION('',(0.,0.,1.));
#7162=DIRECTION('',(1.,0.,0.));
#7163=DIRECTION('',(0.,0.,1.));
#7164=DIRECTION('',(1.,0.,0.));
#7165=DIRECTION('',(0.,0.,1.));
#7166=DIRECTION('',(1.,0.,0.));
#7167=DIRECTION('',(0.,0.,1.));
#7168=DIRECTION('',(1.,0.,0.));
#7169=DIRECTION('',(0.,-1.,2.22044604925031E-16));
#7170=DIRECTION('',(1.,0.,0.));
#7171=DIRECTION('',(0.,-1.,2.22044604925031E-16));
#7172=DIRECTION('',(1.,0.,0.));
#7173=DIRECTION('',(0.,0.,1.));
#7174=DIRECTION('',(1.,0.,0.));
#7175=DIRECTION('',(0.,-1.,2.22044604925031E-16));
#7176=DIRECTION('',(1.,0.,0.));
#7177=DIRECTION('',(0.,-1.,2.22044604925031E-16));
#7178=DIRECTION('',(1.,0.,0.));
#7179=DIRECTION('',(0.,0.,1.));
#7180=DIRECTION('',(2.22044604925031E-16,-1.,0.));
#7181=DIRECTION('',(0.,0.,1.));
#7182=DIRECTION('',(-1.,1.22464679914735E-16,0.));
#7183=DIRECTION('',(0.,0.,1.));
#7184=DIRECTION('',(-1.,1.22464679914735E-16,0.));
#7185=DIRECTION('',(0.,0.,1.));
#7186=DIRECTION('',(-1.,1.22464679914735E-16,0.));
#7187=DIRECTION('',(0.,0.,1.));
#7188=DIRECTION('',(-1.,1.22464679914735E-16,0.));
#7189=DIRECTION('',(0.,0.,1.));
#7190=DIRECTION('',(1.,0.,0.));
#7191=DIRECTION('',(0.,0.,1.));
#7192=DIRECTION('',(1.,0.,0.));
#7193=DIRECTION('',(0.,0.,1.));
#7194=DIRECTION('',(1.,0.,0.));
#7195=DIRECTION('',(0.,0.,1.));
#7196=DIRECTION('',(1.,0.,0.));
#7197=DIRECTION('axis',(0.,0.,1.));
#7198=DIRECTION('refdir',(1.,0.,0.));
#7199=DIRECTION('center_axis',(0.866025403784439,0.,-0.5));
#7200=DIRECTION('ref_axis',(0.5,0.,0.866025403784439));
#7201=DIRECTION('',(0.5,0.,0.866025403784439));
#7202=DIRECTION('',(0.,-1.,0.));
#7203=DIRECTION('',(0.5,0.,0.866025403784439));
#7204=DIRECTION('',(0.,-1.,0.));
#7205=DIRECTION('center_axis',(1.92296268638356E-16,0.,-1.));
#7206=DIRECTION('ref_axis',(1.,0.,1.92296268638356E-16));
#7207=DIRECTION('',(1.,0.,1.92296268638356E-16));
#7208=DIRECTION('',(0.,-1.,0.));
#7209=DIRECTION('',(1.,0.,1.92296268638356E-16));
#7210=DIRECTION('center_axis',(-0.866025403784439,0.,-0.5));
#7211=DIRECTION('ref_axis',(0.5,0.,-0.866025403784439));
#7212=DIRECTION('',(0.5,0.,-0.866025403784439));
#7213=DIRECTION('',(0.,-1.,0.));
#7214=DIRECTION('',(0.5,0.,-0.866025403784438));
#7215=DIRECTION('center_axis',(-0.866025403784439,0.,0.5));
#7216=DIRECTION('ref_axis',(-0.5,0.,-0.866025403784439));
#7217=DIRECTION('',(-0.5,0.,-0.866025403784439));
#7218=DIRECTION('',(0.,-1.,0.));
#7219=DIRECTION('',(-0.5,0.,-0.866025403784439));
#7220=DIRECTION('center_axis',(-1.92296268638356E-16,0.,1.));
#7221=DIRECTION('ref_axis',(-1.,0.,-1.92296268638356E-16));
#7222=DIRECTION('',(-1.,0.,-1.92296268638356E-16));
#7223=DIRECTION('',(0.,-1.,0.));
#7224=DIRECTION('',(-1.,0.,-1.92296268638356E-16));
#7225=DIRECTION('center_axis',(0.866025403784439,0.,0.5));
#7226=DIRECTION('ref_axis',(-0.5,0.,0.866025403784439));
#7227=DIRECTION('',(-0.5,0.,0.866025403784439));
#7228=DIRECTION('',(-0.5,0.,0.866025403784439));
#7229=DIRECTION('center_axis',(0.,-1.,0.));
#7230=DIRECTION('ref_axis',(0.,0.,-1.));
#7231=DIRECTION('center_axis',(0.,1.,0.));
#7232=DIRECTION('ref_axis',(0.,0.,1.));
#7233=DIRECTION('center_axis',(0.,-1.,0.));
#7234=DIRECTION('ref_axis',(1.,0.,0.));
#7235=DIRECTION('center_axis',(0.,-1.,0.));
#7236=DIRECTION('ref_axis',(1.,0.,0.));
#7237=DIRECTION('center_axis',(0.,-1.,0.));
#7238=DIRECTION('ref_axis',(1.,0.,0.));
#7239=DIRECTION('',(0.707106781186547,0.707106781186548,8.65956056235493E-17));
#7240=DIRECTION('center_axis',(0.,-1.,0.));
#7241=DIRECTION('ref_axis',(1.,0.,0.));
#7242=DIRECTION('center_axis',(0.,1.,0.));
#7243=DIRECTION('ref_axis',(1.,0.,0.));
#7244=DIRECTION('',(0.,1.,0.));
#7245=DIRECTION('center_axis',(0.,1.,0.));
#7246=DIRECTION('ref_axis',(1.,0.,0.));
#7247=DIRECTION('center_axis',(0.,-1.,0.));
#7248=DIRECTION('ref_axis',(1.,0.,0.));
#7249=DIRECTION('',(-0.707106781186547,0.707106781186548,-8.65956056235493E-17));
#7250=DIRECTION('center_axis',(0.,-1.,0.));
#7251=DIRECTION('ref_axis',(0.,0.,-1.));
#7252=DIRECTION('axis',(0.,0.,1.));
#7253=DIRECTION('refdir',(1.,0.,0.));
#7254=DIRECTION('center_axis',(1.,0.,0.));
#7255=DIRECTION('ref_axis',(0.,0.,-1.));
#7256=DIRECTION('',(0.,-0.707106781186547,-0.707106781186548));
#7257=DIRECTION('',(0.,-1.,0.));
#7258=DIRECTION('',(0.,-0.707106781186547,0.707106781186548));
#7259=DIRECTION('',(0.,0.,1.));
#7260=DIRECTION('',(0.,0.707106781186547,0.707106781186548));
#7261=DIRECTION('',(0.,1.,0.));
#7262=DIRECTION('',(0.,0.707106781186547,-0.707106781186548));
#7263=DIRECTION('',(0.,0.,-1.));
#7264=DIRECTION('center_axis',(0.,0.707106781186548,-0.707106781186547));
#7265=DIRECTION('ref_axis',(-1.,0.,0.));
#7266=DIRECTION('',(1.,0.,0.));
#7267=DIRECTION('',(0.,-0.707106781186547,-0.707106781186548));
#7268=DIRECTION('',(-1.,0.,0.));
#7269=DIRECTION('center_axis',(0.,1.,0.));
#7270=DIRECTION('ref_axis',(-1.,0.,0.));
#7271=DIRECTION('',(-1.,0.,0.));
#7272=DIRECTION('',(0.,0.,-1.));
#7273=DIRECTION('center_axis',(0.,0.707106781186548,0.707106781186547));
#7274=DIRECTION('ref_axis',(1.,0.,0.));
#7275=DIRECTION('',(1.,0.,0.));
#7276=DIRECTION('',(0.,0.707106781186547,-0.707106781186548));
#7277=DIRECTION('center_axis',(0.,0.,1.));
#7278=DIRECTION('ref_axis',(1.,0.,0.));
#7279=DIRECTION('',(-1.,0.,0.));
#7280=DIRECTION('',(0.,1.,0.));
#7281=DIRECTION('center_axis',(1.,0.,0.));
#7282=DIRECTION('ref_axis',(0.,0.,-1.));
#7283=DIRECTION('',(0.,-0.707106781186547,0.707106781186548));
#7284=DIRECTION('',(0.,-1.,0.));
#7285=DIRECTION('',(0.,0.707106781186547,0.707106781186548));
#7286=DIRECTION('',(0.,0.,1.));
#7287=DIRECTION('center_axis',(0.,0.,1.));
#7288=DIRECTION('ref_axis',(1.,0.,0.));
#7289=DIRECTION('',(1.,0.,0.));
#7290=DIRECTION('center_axis',(0.,-0.707106781186548,0.707106781186547));
#7291=DIRECTION('ref_axis',(1.,0.,0.));
#7292=DIRECTION('',(1.,0.,0.));
#7293=DIRECTION('center_axis',(0.,-0.707106781186548,-0.707106781186547));
#7294=DIRECTION('ref_axis',(-1.,0.,0.));
#7295=DIRECTION('',(-1.,0.,0.));
#7296=DIRECTION('center_axis',(0.,-1.,0.));
#7297=DIRECTION('ref_axis',(1.,0.,0.));
#7298=DIRECTION('axis',(0.,0.,1.));
#7299=DIRECTION('refdir',(1.,0.,0.));
#7300=DIRECTION('center_axis',(0.,1.,0.));
#7301=DIRECTION('ref_axis',(0.,0.,1.));
#7302=DIRECTION('center_axis',(0.,-1.,0.));
#7303=DIRECTION('ref_axis',(1.,0.,0.));
#7304=DIRECTION('center_axis',(0.,-1.,0.));
#7305=DIRECTION('ref_axis',(1.,0.,0.));
#7306=DIRECTION('center_axis',(0.,-1.,0.));
#7307=DIRECTION('ref_axis',(1.,0.,0.));
#7308=DIRECTION('',(0.707106781186548,0.707106781186547,8.65956056235493E-17));
#7309=DIRECTION('center_axis',(0.,-1.,0.));
#7310=DIRECTION('ref_axis',(1.,0.,0.));
#7311=DIRECTION('center_axis',(0.,-1.,0.));
#7312=DIRECTION('ref_axis',(1.,0.,0.));
#7313=DIRECTION('',(0.,1.,0.));
#7314=DIRECTION('center_axis',(0.,1.,0.));
#7315=DIRECTION('ref_axis',(1.,0.,0.));
#7316=DIRECTION('center_axis',(0.,-1.,0.));
#7317=DIRECTION('ref_axis',(1.,0.,0.));
#7318=DIRECTION('',(-0.707106781186547,0.707106781186548,-8.65956056235493E-17));
#7319=DIRECTION('center_axis',(0.,-1.,0.));
#7320=DIRECTION('ref_axis',(0.,0.,-1.));
#7321=DIRECTION('center_axis',(0.,-1.,0.));
#7322=DIRECTION('ref_axis',(1.,0.,0.));
#7323=DIRECTION('center_axis',(0.,1.,0.));
#7324=DIRECTION('ref_axis',(1.,0.,0.));
#7325=DIRECTION('center_axis',(0.,1.,0.));
#7326=DIRECTION('ref_axis',(1.,0.,0.));
#7327=DIRECTION('',(-0.447213595499958,0.894427190999916,-5.47678698264203E-17));
#7328=DIRECTION('center_axis',(0.,-1.,0.));
#7329=DIRECTION('ref_axis',(1.,0.,0.));
#7330=DIRECTION('center_axis',(0.,1.,0.));
#7331=DIRECTION('ref_axis',(1.,0.,0.));
#7332=DIRECTION('',(0.,1.,0.));
#7333=DIRECTION('center_axis',(0.,1.,0.));
#7334=DIRECTION('ref_axis',(1.,0.,0.));
#7335=DIRECTION('center_axis',(0.,-1.,0.));
#7336=DIRECTION('ref_axis',(1.,0.,0.));
#7337=DIRECTION('',(-0.707106781186547,0.707106781186548,-8.65956056235493E-17));
#7338=DIRECTION('center_axis',(0.,-1.,0.));
#7339=DIRECTION('ref_axis',(0.,0.,-1.));
#7340=DIRECTION('center_axis',(0.866025403784439,0.,-0.5));
#7341=DIRECTION('ref_axis',(0.5,0.,0.866025403784439));
#7342=DIRECTION('',(-0.5,0.,-0.866025403784439));
#7343=DIRECTION('',(0.,-1.,0.));
#7344=DIRECTION('',(0.5,0.,0.866025403784439));
#7345=DIRECTION('',(0.,-1.,0.));
#7346=DIRECTION('center_axis',(1.20185167898973E-16,0.,-1.));
#7347=DIRECTION('ref_axis',(1.,0.,1.20185167898973E-16));
#7348=DIRECTION('',(-1.,0.,-1.20185167898973E-16));
#7349=DIRECTION('',(0.,-1.,0.));
#7350=DIRECTION('',(1.,0.,1.20185167898973E-16));
#7351=DIRECTION('center_axis',(-0.866025403784439,0.,-0.5));
#7352=DIRECTION('ref_axis',(0.5,0.,-0.866025403784439));
#7353=DIRECTION('',(-0.5,0.,0.866025403784439));
#7354=DIRECTION('',(0.,-1.,0.));
#7355=DIRECTION('',(0.5,0.,-0.866025403784439));
#7356=DIRECTION('center_axis',(-0.866025403784439,0.,0.5));
#7357=DIRECTION('ref_axis',(-0.5,0.,-0.866025403784439));
#7358=DIRECTION('',(0.5,0.,0.866025403784439));
#7359=DIRECTION('',(0.,-1.,0.));
#7360=DIRECTION('',(-0.5,0.,-0.866025403784439));
#7361=DIRECTION('center_axis',(-2.40370335797945E-16,0.,1.));
#7362=DIRECTION('ref_axis',(-1.,0.,-2.40370335797945E-16));
#7363=DIRECTION('',(1.,0.,2.40370335797945E-16));
#7364=DIRECTION('',(0.,-1.,0.));
#7365=DIRECTION('',(-1.,0.,-2.40370335797945E-16));
#7366=DIRECTION('center_axis',(0.866025403784439,0.,0.5));
#7367=DIRECTION('ref_axis',(-0.5,0.,0.866025403784439));
#7368=DIRECTION('',(0.5,0.,-0.866025403784439));
#7369=DIRECTION('',(-0.5,0.,0.866025403784439));
#7370=DIRECTION('center_axis',(0.,1.,0.));
#7371=DIRECTION('ref_axis',(1.,0.,0.));
#7372=DIRECTION('center_axis',(0.,-1.,0.));
#7373=DIRECTION('ref_axis',(0.,0.,-1.));
#7374=DIRECTION('',(0.,0.,1.));
#7375=DIRECTION('',(1.,0.,0.));
#7376=DIRECTION('',(0.,0.,1.));
#7377=DIRECTION('',(1.,0.,0.));
#7378=DIRECTION('',(0.,0.,1.));
#7379=DIRECTION('',(1.,0.,0.));
#7380=DIRECTION('',(0.,0.,1.));
#7381=DIRECTION('',(1.,0.,0.));
#7382=DIRECTION('',(0.,0.,1.));
#7383=DIRECTION('',(1.,0.,0.));
#7384=DIRECTION('',(0.,0.,1.));
#7385=DIRECTION('',(1.,0.,0.));
#7386=DIRECTION('',(0.,-1.,2.22044604925031E-16));
#7387=DIRECTION('',(1.,0.,0.));
#7388=DIRECTION('',(8.65956056235493E-17,-8.65956056235493E-17,-1.));
#7389=DIRECTION('',(2.22044604925031E-16,1.,-8.65956056235494E-17));
#7390=DIRECTION('',(0.,0.,1.));
#7391=DIRECTION('',(1.,0.,0.));
#7392=DIRECTION('',(0.,0.,1.));
#7393=DIRECTION('',(1.,0.,0.));
#7394=DIRECTION('',(0.,0.,1.));
#7395=DIRECTION('',(1.,0.,0.));
#7396=CARTESIAN_POINT('',(0.,0.,0.));
#7397=CARTESIAN_POINT('',(0.,0.,0.));
#7398=CARTESIAN_POINT('',(0.,0.,0.));
#7399=CARTESIAN_POINT('Origin',(3.8,1.,-0.1));
#7400=CARTESIAN_POINT('',(3.55,1.,0.));
#7401=CARTESIAN_POINT('Origin',(3.8,1.,0.));
#7402=CARTESIAN_POINT('',(3.55,1.,1.));
#7403=CARTESIAN_POINT('',(3.55,1.,-0.1));
#7404=CARTESIAN_POINT('Origin',(3.8,1.,1.));
#7405=CARTESIAN_POINT('Origin',(-3.8,5.,-0.1));
#7406=CARTESIAN_POINT('',(-4.05,5.,0.));
#7407=CARTESIAN_POINT('Origin',(-3.8,5.,0.));
#7408=CARTESIAN_POINT('',(-4.05,5.,1.));
#7409=CARTESIAN_POINT('',(-4.05,5.,-0.1));
#7410=CARTESIAN_POINT('Origin',(-3.8,5.,1.));
#7411=CARTESIAN_POINT('Origin',(-3.8,1.,-0.1));
#7412=CARTESIAN_POINT('',(-4.05,1.,0.));
#7413=CARTESIAN_POINT('Origin',(-3.8,1.,0.));
#7414=CARTESIAN_POINT('',(-4.05,1.,1.));
#7415=CARTESIAN_POINT('',(-4.05,1.,-0.1));
#7416=CARTESIAN_POINT('Origin',(-3.8,1.,1.));
#7417=CARTESIAN_POINT('Origin',(3.8,5.,-0.1));
#7418=CARTESIAN_POINT('',(3.55,5.,0.));
#7419=CARTESIAN_POINT('Origin',(3.8,5.,0.));
#7420=CARTESIAN_POINT('',(3.55,5.,1.));
#7421=CARTESIAN_POINT('',(3.55,5.,-0.1));
#7422=CARTESIAN_POINT('Origin',(3.8,5.,1.));
#7423=CARTESIAN_POINT('Origin',(5.5,7.,0.));
#7424=CARTESIAN_POINT('',(5.5,7.,0.));
#7425=CARTESIAN_POINT('',(-5.5,7.,0.));
#7426=CARTESIAN_POINT('',(5.5,7.,0.));
#7427=CARTESIAN_POINT('',(-5.5,7.,1.));
#7428=CARTESIAN_POINT('',(-5.5,7.,0.));
#7429=CARTESIAN_POINT('',(5.5,7.,1.));
#7430=CARTESIAN_POINT('',(5.5,7.,1.));
#7431=CARTESIAN_POINT('',(5.5,7.,0.));
#7432=CARTESIAN_POINT('Origin',(5.5,-1.,0.));
#7433=CARTESIAN_POINT('',(5.5,-1.,0.));
#7434=CARTESIAN_POINT('',(5.5,-1.,0.));
#7435=CARTESIAN_POINT('',(5.5,-1.,1.));
#7436=CARTESIAN_POINT('',(5.5,-1.,1.));
#7437=CARTESIAN_POINT('',(5.5,-1.,0.));
#7438=CARTESIAN_POINT('Origin',(-5.5,-1.,0.));
#7439=CARTESIAN_POINT('',(-5.5,-1.,0.));
#7440=CARTESIAN_POINT('',(-5.5,-1.,0.));
#7441=CARTESIAN_POINT('',(-5.5,-1.,1.));
#7442=CARTESIAN_POINT('',(-5.5,-1.,1.));
#7443=CARTESIAN_POINT('',(-5.5,-1.,0.));
#7444=CARTESIAN_POINT('Origin',(-5.5,7.,0.));
#7445=CARTESIAN_POINT('',(-5.5,7.,0.));
#7446=CARTESIAN_POINT('',(-5.5,7.,1.));
#7447=CARTESIAN_POINT('Origin',(0.,3.,1.));
#7448=CARTESIAN_POINT('Origin',(0.,3.,0.));
#7449=CARTESIAN_POINT('',(0.,0.,0.));
#7450=CARTESIAN_POINT('Origin',(-2.8,4.4,4.5));
#7451=CARTESIAN_POINT('',(-2.965,4.4,4.5));
#7452=CARTESIAN_POINT('Origin',(-2.8,4.4,4.5));
#7453=CARTESIAN_POINT('',(-2.965,6.,4.5));
#7454=CARTESIAN_POINT('',(-2.965,4.4,4.5));
#7455=CARTESIAN_POINT('Origin',(-2.8,6.,4.5));
#7456=CARTESIAN_POINT('Origin',(-2.8,4.4,4.5));
#7457=CARTESIAN_POINT('Origin',(1.71450551880629E-16,4.4,7.3));
#7458=CARTESIAN_POINT('',(-0.165,4.4,7.3));
#7459=CARTESIAN_POINT('Origin',(1.71450551880629E-16,4.4,7.3));
#7460=CARTESIAN_POINT('',(-0.165,6.,7.3));
#7461=CARTESIAN_POINT('',(-0.165,4.4,7.3));
#7462=CARTESIAN_POINT('Origin',(1.71450551880629E-16,6.,7.3));
#7463=CARTESIAN_POINT('Origin',(1.66533453693773E-16,4.4,7.3));
#7464=CARTESIAN_POINT('Origin',(2.8,4.4,4.5));
#7465=CARTESIAN_POINT('',(2.635,4.4,4.5));
#7466=CARTESIAN_POINT('Origin',(2.8,4.4,4.5));
#7467=CARTESIAN_POINT('',(2.635,6.,4.5));
#7468=CARTESIAN_POINT('',(2.635,4.4,4.5));
#7469=CARTESIAN_POINT('Origin',(2.8,6.,4.5));
#7470=CARTESIAN_POINT('Origin',(2.8,4.4,4.5));
#7471=CARTESIAN_POINT('Origin',(-5.14351655641888E-16,4.4,1.7));
#7472=CARTESIAN_POINT('',(-0.165000000000001,4.4,1.7));
#7473=CARTESIAN_POINT('Origin',(-5.14351655641888E-16,4.4,1.7));
#7474=CARTESIAN_POINT('',(-0.165000000000001,6.,1.7));
#7475=CARTESIAN_POINT('',(-0.165000000000001,4.4,1.7));
#7476=CARTESIAN_POINT('Origin',(-5.14351655641888E-16,6.,1.7));
#7477=CARTESIAN_POINT('Origin',(-5.27355936696949E-16,4.4,1.7));
#7478=CARTESIAN_POINT('Origin',(-2.8,-0.1,4.5));
#7479=CARTESIAN_POINT('',(-2.965,0.,4.5));
#7480=CARTESIAN_POINT('Origin',(-2.8,0.,4.5));
#7481=CARTESIAN_POINT('',(-2.965,1.6,4.5));
#7482=CARTESIAN_POINT('',(-2.965,-0.1,4.5));
#7483=CARTESIAN_POINT('Origin',(-2.8,1.6,4.5));
#7484=CARTESIAN_POINT('Origin',(-2.8,1.6,4.5));
#7485=CARTESIAN_POINT('Origin',(1.71450551880629E-16,-0.1,7.3));
#7486=CARTESIAN_POINT('',(-0.165,0.,7.3));
#7487=CARTESIAN_POINT('Origin',(1.71450551880629E-16,0.,7.3));
#7488=CARTESIAN_POINT('',(-0.165,1.6,7.3));
#7489=CARTESIAN_POINT('',(-0.165,-0.1,7.3));
#7490=CARTESIAN_POINT('Origin',(1.71450551880629E-16,1.6,7.3));
#7491=CARTESIAN_POINT('Origin',(1.66533453693773E-16,1.6,7.3));
#7492=CARTESIAN_POINT('Origin',(2.8,-0.1,4.5));
#7493=CARTESIAN_POINT('',(2.635,0.,4.5));
#7494=CARTESIAN_POINT('Origin',(2.8,0.,4.5));
#7495=CARTESIAN_POINT('',(2.635,1.6,4.5));
#7496=CARTESIAN_POINT('',(2.635,-0.1,4.5));
#7497=CARTESIAN_POINT('Origin',(2.8,1.6,4.5));
#7498=CARTESIAN_POINT('Origin',(2.8,1.6,4.5));
#7499=CARTESIAN_POINT('Origin',(-5.14351655641888E-16,-0.1,1.7));
#7500=CARTESIAN_POINT('',(-0.165000000000001,0.,1.7));
#7501=CARTESIAN_POINT('Origin',(-5.14351655641888E-16,0.,1.7));
#7502=CARTESIAN_POINT('',(-0.165000000000001,1.6,1.7));
#7503=CARTESIAN_POINT('',(-0.165000000000001,-0.1,1.7));
#7504=CARTESIAN_POINT('Origin',(-5.14351655641888E-16,1.6,1.7));
#7505=CARTESIAN_POINT('Origin',(-5.27355936696949E-16,1.6,1.7));
#7506=CARTESIAN_POINT('Origin',(2.1,3.,4.5));
#7507=CARTESIAN_POINT('',(2.24794906525926,3.,3.815));
#7508=CARTESIAN_POINT('',(2.24794906525926,3.,5.185));
#7509=CARTESIAN_POINT('Ctrl Pts',(2.24794906525926,3.,3.815));
#7510=CARTESIAN_POINT('Ctrl Pts',(2.24794906525926,3.08656638593426,3.815));
#7511=CARTESIAN_POINT('Ctrl Pts',(2.25347242618579,3.1785329272349,3.83240366255852));
#7512=CARTESIAN_POINT('Ctrl Pts',(2.273052742601,3.34713817113353,3.90246002212197));
#7513=CARTESIAN_POINT('Ctrl Pts',(2.28678795375575,3.42382433348001,3.95508804325444));
#7514=CARTESIAN_POINT('Ctrl Pts',(2.31229010718961,3.54489596201988,4.07615967179431));
#7515=CARTESIAN_POINT('Ctrl Pts',(2.32576600179013,3.59753638520302,4.15285236357336));
#7516=CARTESIAN_POINT('Ctrl Pts',(2.34474519428597,3.66760188102413,4.32148123334598));
#7517=CARTESIAN_POINT('Ctrl Pts',(2.35,3.685,4.4134564835475));
#7518=CARTESIAN_POINT('Ctrl Pts',(2.35,3.685,4.5865435164525));
#7519=CARTESIAN_POINT('Ctrl Pts',(2.34474519428597,3.66760188102413,4.67851876665402));
#7520=CARTESIAN_POINT('Ctrl Pts',(2.32576600179013,3.59753638520302,4.84714763642664));
#7521=CARTESIAN_POINT('Ctrl Pts',(2.31229010718961,3.54489596201988,4.92384032820569));
#7522=CARTESIAN_POINT('Ctrl Pts',(2.28678795375575,3.42382433348001,5.04491195674555));
#7523=CARTESIAN_POINT('Ctrl Pts',(2.273052742601,3.34713817113353,5.09753997787803));
#7524=CARTESIAN_POINT('Ctrl Pts',(2.25347242618579,3.1785329272349,5.16759633744148));
#7525=CARTESIAN_POINT('Ctrl Pts',(2.24794906525926,3.08656638593426,5.185));
#7526=CARTESIAN_POINT('Ctrl Pts',(2.24794906525926,3.,5.185));
#7527=CARTESIAN_POINT('Ctrl Pts',(2.24794906525926,3.,5.185));
#7528=CARTESIAN_POINT('Ctrl Pts',(2.24794906525926,2.91343361406574,5.185));
#7529=CARTESIAN_POINT('Ctrl Pts',(2.25347242618579,2.8214670727651,5.16759633744148));
#7530=CARTESIAN_POINT('Ctrl Pts',(2.273052742601,2.65286182886647,5.09753997787803));
#7531=CARTESIAN_POINT('Ctrl Pts',(2.28678795375575,2.57617566651999,5.04491195674556));
#7532=CARTESIAN_POINT('Ctrl Pts',(2.31229010718961,2.45510403798012,4.92384032820569));
#7533=CARTESIAN_POINT('Ctrl Pts',(2.32576600179013,2.40246361479698,4.84714763642664));
#7534=CARTESIAN_POINT('Ctrl Pts',(2.34474519428597,2.33239811897587,4.67851876665402));
#7535=CARTESIAN_POINT('Ctrl Pts',(2.35,2.315,4.5865435164525));
#7536=CARTESIAN_POINT('Ctrl Pts',(2.35,2.315,4.4134564835475));
#7537=CARTESIAN_POINT('Ctrl Pts',(2.34474519428597,2.33239811897587,4.32148123334598));
#7538=CARTESIAN_POINT('Ctrl Pts',(2.32576600179013,2.40246361479698,4.15285236357336));
#7539=CARTESIAN_POINT('Ctrl Pts',(2.31229010718961,2.45510403798012,4.07615967179431));
#7540=CARTESIAN_POINT('Ctrl Pts',(2.28678795375575,2.57617566651999,3.95508804325444));
#7541=CARTESIAN_POINT('Ctrl Pts',(2.273052742601,2.65286182886647,3.90246002212197));
#7542=CARTESIAN_POINT('Ctrl Pts',(2.25347242618579,2.8214670727651,3.83240366255852));
#7543=CARTESIAN_POINT('Ctrl Pts',(2.24794906525926,2.91343361406574,3.815));
#7544=CARTESIAN_POINT('Ctrl Pts',(2.24794906525926,3.,3.815));
#7545=CARTESIAN_POINT('',(3.43231335982017,3.,5.185));
#7546=CARTESIAN_POINT('',(2.1,3.,5.185));
#7547=CARTESIAN_POINT('',(3.43231335982017,3.,3.815));
#7548=CARTESIAN_POINT('Ctrl Pts',(3.43231335982017,3.,3.815));
#7549=CARTESIAN_POINT('Ctrl Pts',(3.43231335982017,2.91374778588775,3.815));
#7550=CARTESIAN_POINT('Ctrl Pts',(3.43590159793026,2.82190332857989,3.83228322178306));
#7551=CARTESIAN_POINT('Ctrl Pts',(3.44876354740763,2.65320224067205,3.90225803271408));
#7552=CARTESIAN_POINT('Ctrl Pts',(3.45784079740304,2.57632582235222,3.95493788742221));
#7553=CARTESIAN_POINT('Ctrl Pts',(3.47480256335419,2.45494100103992,4.07632270873451));
#7554=CARTESIAN_POINT('Ctrl Pts',(3.48380333962794,2.40225870697367,4.15320045129105));
#7555=CARTESIAN_POINT('Ctrl Pts',(3.49648941236884,2.33228212593366,4.3219061343655));
#7556=CARTESIAN_POINT('Ctrl Pts',(3.5,2.315,4.41375221065075));
#7557=CARTESIAN_POINT('Ctrl Pts',(3.5,2.315,4.58624778934925));
#7558=CARTESIAN_POINT('Ctrl Pts',(3.49648941236884,2.33228212593366,4.6780938656345));
#7559=CARTESIAN_POINT('Ctrl Pts',(3.48380333962794,2.40225870697367,4.84679954870895));
#7560=CARTESIAN_POINT('Ctrl Pts',(3.47480256335419,2.45494100103992,4.92367729126549));
#7561=CARTESIAN_POINT('Ctrl Pts',(3.45784079740304,2.57632582235222,5.04506211257779));
#7562=CARTESIAN_POINT('Ctrl Pts',(3.44876354740763,2.65320224067205,5.09774196728592));
#7563=CARTESIAN_POINT('Ctrl Pts',(3.43590159793026,2.82190332857989,5.16771677821694));
#7564=CARTESIAN_POINT('Ctrl Pts',(3.43231335982017,2.91374778588775,5.185));
#7565=CARTESIAN_POINT('Ctrl Pts',(3.43231335982017,3.,5.185));
#7566=CARTESIAN_POINT('Ctrl Pts',(3.43231335982017,3.,5.185));
#7567=CARTESIAN_POINT('Ctrl Pts',(3.43231335982017,3.08625221411225,5.185));
#7568=CARTESIAN_POINT('Ctrl Pts',(3.43590159793026,3.17809667142011,5.16771677821694));
#7569=CARTESIAN_POINT('Ctrl Pts',(3.44876354740763,3.34679775932795,5.09774196728592));
#7570=CARTESIAN_POINT('Ctrl Pts',(3.45784079740304,3.42367417764778,5.04506211257779));
#7571=CARTESIAN_POINT('Ctrl Pts',(3.47480256335419,3.54505899896008,4.92367729126549));
#7572=CARTESIAN_POINT('Ctrl Pts',(3.48380333962794,3.59774129302633,4.84679954870895));
#7573=CARTESIAN_POINT('Ctrl Pts',(3.49648941236884,3.66771787406634,4.6780938656345));
#7574=CARTESIAN_POINT('Ctrl Pts',(3.5,3.685,4.58624778934925));
#7575=CARTESIAN_POINT('Ctrl Pts',(3.5,3.685,4.41375221065075));
#7576=CARTESIAN_POINT('Ctrl Pts',(3.49648941236884,3.66771787406634,4.3219061343655));
#7577=CARTESIAN_POINT('Ctrl Pts',(3.48380333962794,3.59774129302633,4.15320045129105));
#7578=CARTESIAN_POINT('Ctrl Pts',(3.47480256335419,3.54505899896008,4.07632270873451));
#7579=CARTESIAN_POINT('Ctrl Pts',(3.45784079740304,3.42367417764778,3.95493788742221));
#7580=CARTESIAN_POINT('Ctrl Pts',(3.44876354740763,3.34679775932795,3.90225803271408));
#7581=CARTESIAN_POINT('Ctrl Pts',(3.43590159793026,3.17809667142011,3.83228322178306));
#7582=CARTESIAN_POINT('Ctrl Pts',(3.43231335982017,3.08625221411225,3.815));
#7583=CARTESIAN_POINT('Ctrl Pts',(3.43231335982017,3.,3.815));
#7584=CARTESIAN_POINT('Origin',(3.8,1.,0.9));
#7585=CARTESIAN_POINT('',(3.47,1.,1.));
#7586=CARTESIAN_POINT('Origin',(3.8,1.,1.));
#7587=CARTESIAN_POINT('',(3.47,1.,2.5));
#7588=CARTESIAN_POINT('',(3.47,1.,0.9));
#7589=CARTESIAN_POINT('Origin',(3.8,1.,2.5));
#7590=CARTESIAN_POINT('Origin',(-3.8,5.,0.9));
#7591=CARTESIAN_POINT('',(-4.13,5.,1.));
#7592=CARTESIAN_POINT('Origin',(-3.8,5.,1.));
#7593=CARTESIAN_POINT('',(-4.13,5.,2.5));
#7594=CARTESIAN_POINT('',(-4.13,5.,0.9));
#7595=CARTESIAN_POINT('Origin',(-3.8,5.,2.5));
#7596=CARTESIAN_POINT('Origin',(-3.8,1.,0.9));
#7597=CARTESIAN_POINT('',(-4.13,1.,1.));
#7598=CARTESIAN_POINT('Origin',(-3.8,1.,1.));
#7599=CARTESIAN_POINT('',(-4.13,1.,2.5));
#7600=CARTESIAN_POINT('',(-4.13,1.,0.9));
#7601=CARTESIAN_POINT('Origin',(-3.8,1.,2.5));
#7602=CARTESIAN_POINT('Origin',(3.8,5.,0.9));
#7603=CARTESIAN_POINT('',(3.47,5.,1.));
#7604=CARTESIAN_POINT('Origin',(3.8,5.,1.));
#7605=CARTESIAN_POINT('',(3.47,5.,2.5));
#7606=CARTESIAN_POINT('',(3.47,5.,0.9));
#7607=CARTESIAN_POINT('Origin',(3.8,5.,2.5));
#7608=CARTESIAN_POINT('Origin',(0.,5.5,1.75));
#7609=CARTESIAN_POINT('',(2.87228132326901,5.5,2.5));
#7610=CARTESIAN_POINT('',(0.,5.5,1.));
#7611=CARTESIAN_POINT('Origin',(0.,5.5,4.5));
#7612=CARTESIAN_POINT('',(4.5,5.5,2.5));
#7613=CARTESIAN_POINT('',(4.5,5.5,2.5));
#7614=CARTESIAN_POINT('',(4.5,5.5,1.));
#7615=CARTESIAN_POINT('',(4.5,5.5,1.));
#7616=CARTESIAN_POINT('',(-4.5,5.5,1.));
#7617=CARTESIAN_POINT('Origin',(0.,5.5,1.75));
#7618=CARTESIAN_POINT('',(-2.87228132326901,5.5,2.5));
#7619=CARTESIAN_POINT('Origin',(0.,5.5,4.5));
#7620=CARTESIAN_POINT('',(-4.5,5.5,1.));
#7621=CARTESIAN_POINT('',(-4.5,5.5,1.));
#7622=CARTESIAN_POINT('',(-4.5,5.5,2.5));
#7623=CARTESIAN_POINT('',(-4.5,5.5,2.5));
#7624=CARTESIAN_POINT('',(4.5,5.5,2.5));
#7625=CARTESIAN_POINT('Origin',(0.,4.5,1.75));
#7626=CARTESIAN_POINT('',(0.,4.5,1.));
#7627=CARTESIAN_POINT('',(2.87228132326901,4.5,2.5));
#7628=CARTESIAN_POINT('Origin',(0.,4.5,4.5));
#7629=CARTESIAN_POINT('',(4.5,4.5,1.));
#7630=CARTESIAN_POINT('',(-4.5,4.5,1.));
#7631=CARTESIAN_POINT('',(4.5,4.5,2.5));
#7632=CARTESIAN_POINT('',(4.5,4.5,1.));
#7633=CARTESIAN_POINT('',(4.5,4.5,2.5));
#7634=CARTESIAN_POINT('Origin',(0.,4.5,1.75));
#7635=CARTESIAN_POINT('',(-2.87228132326901,4.5,2.5));
#7636=CARTESIAN_POINT('Origin',(0.,4.5,4.5));
#7637=CARTESIAN_POINT('',(-4.5,4.5,2.5));
#7638=CARTESIAN_POINT('',(4.5,4.5,2.5));
#7639=CARTESIAN_POINT('',(-4.5,4.5,1.));
#7640=CARTESIAN_POINT('',(-4.5,4.5,2.5));
#7641=CARTESIAN_POINT('',(-4.5,4.5,1.));
#7642=CARTESIAN_POINT('Origin',(-4.5,4.5,2.5));
#7643=CARTESIAN_POINT('',(2.87228132326901,0.,2.5));
#7644=CARTESIAN_POINT('',(4.5,4.5,2.5));
#7645=CARTESIAN_POINT('Origin',(-4.5,4.5,2.5));
#7646=CARTESIAN_POINT('',(-2.87228132326901,0.,2.5));
#7647=CARTESIAN_POINT('',(-4.5,4.5,2.5));
#7648=CARTESIAN_POINT('Origin',(-4.5,4.5,1.));
#7649=CARTESIAN_POINT('',(-4.5,4.5,1.));
#7650=CARTESIAN_POINT('Origin',(4.5,4.5,1.));
#7651=CARTESIAN_POINT('',(4.5,4.5,1.));
#7652=CARTESIAN_POINT('Origin',(4.5,4.5,2.5));
#7653=CARTESIAN_POINT('Origin',(0.,1.5,1.75));
#7654=CARTESIAN_POINT('',(2.87228132326901,1.5,2.5));
#7655=CARTESIAN_POINT('',(0.,1.5,1.));
#7656=CARTESIAN_POINT('Origin',(0.,1.5,4.5));
#7657=CARTESIAN_POINT('',(4.5,1.5,2.5));
#7658=CARTESIAN_POINT('',(4.5,1.5,2.5));
#7659=CARTESIAN_POINT('',(4.5,1.5,1.));
#7660=CARTESIAN_POINT('',(4.5,1.5,1.));
#7661=CARTESIAN_POINT('',(-4.5,1.5,1.));
#7662=CARTESIAN_POINT('Origin',(0.,1.5,1.75));
#7663=CARTESIAN_POINT('',(-2.87228132326901,1.5,2.5));
#7664=CARTESIAN_POINT('Origin',(0.,1.5,4.5));
#7665=CARTESIAN_POINT('',(-4.5,1.5,1.));
#7666=CARTESIAN_POINT('',(-4.5,1.5,1.));
#7667=CARTESIAN_POINT('',(-4.5,1.5,2.5));
#7668=CARTESIAN_POINT('',(-4.5,1.5,2.5));
#7669=CARTESIAN_POINT('',(4.5,1.5,2.5));
#7670=CARTESIAN_POINT('Origin',(0.,0.5,1.75));
#7671=CARTESIAN_POINT('',(0.,0.5,1.));
#7672=CARTESIAN_POINT('',(2.87228132326901,0.5,2.5));
#7673=CARTESIAN_POINT('Origin',(0.,0.5,4.5));
#7674=CARTESIAN_POINT('',(4.5,0.5,1.));
#7675=CARTESIAN_POINT('',(-4.5,0.5,1.));
#7676=CARTESIAN_POINT('',(4.5,0.5,2.5));
#7677=CARTESIAN_POINT('',(4.5,0.5,1.));
#7678=CARTESIAN_POINT('',(4.5,0.5,2.5));
#7679=CARTESIAN_POINT('Origin',(0.,0.5,1.75));
#7680=CARTESIAN_POINT('',(-2.87228132326901,0.5,2.5));
#7681=CARTESIAN_POINT('Origin',(0.,0.5,4.5));
#7682=CARTESIAN_POINT('',(-4.5,0.5,2.5));
#7683=CARTESIAN_POINT('',(4.5,0.5,2.5));
#7684=CARTESIAN_POINT('',(-4.5,0.5,1.));
#7685=CARTESIAN_POINT('',(-4.5,0.5,2.5));
#7686=CARTESIAN_POINT('',(-4.5,0.5,1.));
#7687=CARTESIAN_POINT('Origin',(-4.5,0.5,2.5));
#7688=CARTESIAN_POINT('',(2.87228132326901,0.,2.5));
#7689=CARTESIAN_POINT('',(4.5,0.5,2.5));
#7690=CARTESIAN_POINT('Origin',(-4.5,0.5,2.5));
#7691=CARTESIAN_POINT('',(-2.87228132326901,0.,2.5));
#7692=CARTESIAN_POINT('',(-4.5,0.5,2.5));
#7693=CARTESIAN_POINT('Origin',(-4.5,0.5,1.));
#7694=CARTESIAN_POINT('',(-4.5,0.5,1.));
#7695=CARTESIAN_POINT('Origin',(4.5,0.5,1.));
#7696=CARTESIAN_POINT('',(4.5,0.5,1.));
#7697=CARTESIAN_POINT('Origin',(4.5,0.5,2.5));
#7698=CARTESIAN_POINT('Origin',(0.,0.,4.5));
#7699=CARTESIAN_POINT('',(-2.35,6.,4.5));
#7700=CARTESIAN_POINT('Origin',(0.,6.,4.5));
#7701=CARTESIAN_POINT('',(-2.35,0.,4.5));
#7702=CARTESIAN_POINT('',(-2.35,0.,4.5));
#7703=CARTESIAN_POINT('Origin',(0.,0.,4.5));
#7704=CARTESIAN_POINT('Origin',(0.,0.,4.5));
#7705=CARTESIAN_POINT('',(-3.5,6.,4.5));
#7706=CARTESIAN_POINT('Origin',(0.,6.,4.5));
#7707=CARTESIAN_POINT('',(-3.5,0.,4.5));
#7708=CARTESIAN_POINT('',(-3.5,0.,4.5));
#7709=CARTESIAN_POINT('Origin',(0.,0.,4.5));
#7710=CARTESIAN_POINT('Origin',(0.,6.,4.5));
#7711=CARTESIAN_POINT('Origin',(0.,0.,4.5));
#7712=CARTESIAN_POINT('',(0.,0.,0.));
#7713=CARTESIAN_POINT('Origin',(0.,1.9,4.5));
#7714=CARTESIAN_POINT('',(-1.16,1.9,4.5));
#7715=CARTESIAN_POINT('Origin',(0.,1.9,4.5));
#7716=CARTESIAN_POINT('',(-1.16,2.2,4.5));
#7717=CARTESIAN_POINT('',(-1.16,1.9,4.5));
#7718=CARTESIAN_POINT('Origin',(0.,2.2,4.5));
#7719=CARTESIAN_POINT('Origin',(0.,2.2,4.5));
#7720=CARTESIAN_POINT('',(-1.005,2.2,4.5));
#7721=CARTESIAN_POINT('Origin',(0.,2.2,4.5));
#7722=CARTESIAN_POINT('Origin',(0.,1.9,4.5));
#7723=CARTESIAN_POINT('',(-1.005,1.9,4.5));
#7724=CARTESIAN_POINT('Origin',(0.,1.9,4.5));
#7725=CARTESIAN_POINT('Origin',(0.,1.7,4.5));
#7726=CARTESIAN_POINT('',(-1.005,1.7,4.5));
#7727=CARTESIAN_POINT('',(-1.005,1.7,4.5));
#7728=CARTESIAN_POINT('Origin',(0.,1.7,4.5));
#7729=CARTESIAN_POINT('Origin',(0.,1.7,4.5));
#7730=CARTESIAN_POINT('',(-1.005,2.4,4.5));
#7731=CARTESIAN_POINT('Origin',(0.,2.4,4.5));
#7732=CARTESIAN_POINT('',(-1.005,1.7,4.5));
#7733=CARTESIAN_POINT('Origin',(0.,1.7,4.5));
#7734=CARTESIAN_POINT('',(-2.34,2.4,4.5));
#7735=CARTESIAN_POINT('Origin',(0.,2.4,4.5));
#7736=CARTESIAN_POINT('',(-2.34,1.7,4.5));
#7737=CARTESIAN_POINT('',(-2.34,1.7,4.5));
#7738=CARTESIAN_POINT('Origin',(0.,1.7,4.5));
#7739=CARTESIAN_POINT('Origin',(0.,2.4,4.5));
#7740=CARTESIAN_POINT('Origin',(0.,1.7,4.5));
#7741=CARTESIAN_POINT('',(0.,0.,0.));
#7742=CARTESIAN_POINT('Origin',(0.,2.05,4.5));
#7743=CARTESIAN_POINT('',(-1.22464679914735E-16,2.05,5.5));
#7744=CARTESIAN_POINT('Origin',(-1.3164953090834E-16,2.05,5.575));
#7745=CARTESIAN_POINT('Origin',(0.,2.05,4.5));
#7746=CARTESIAN_POINT('',(0.,0.,0.));
#7747=CARTESIAN_POINT('Origin',(0.,3.8,4.5));
#7748=CARTESIAN_POINT('',(-1.16,3.8,4.5));
#7749=CARTESIAN_POINT('Origin',(0.,3.8,4.5));
#7750=CARTESIAN_POINT('',(-1.16,4.1,4.5));
#7751=CARTESIAN_POINT('',(-1.16,3.8,4.5));
#7752=CARTESIAN_POINT('Origin',(0.,4.1,4.5));
#7753=CARTESIAN_POINT('Origin',(0.,4.1,4.5));
#7754=CARTESIAN_POINT('',(-1.005,4.1,4.5));
#7755=CARTESIAN_POINT('Origin',(0.,4.1,4.5));
#7756=CARTESIAN_POINT('Origin',(0.,3.8,4.5));
#7757=CARTESIAN_POINT('',(-1.005,3.8,4.5));
#7758=CARTESIAN_POINT('Origin',(0.,3.8,4.5));
#7759=CARTESIAN_POINT('Origin',(0.,3.6,4.5));
#7760=CARTESIAN_POINT('',(-1.005,3.6,4.5));
#7761=CARTESIAN_POINT('',(-1.005,3.6,4.5));
#7762=CARTESIAN_POINT('Origin',(0.,3.6,4.5));
#7763=CARTESIAN_POINT('Origin',(0.,3.6,4.5));
#7764=CARTESIAN_POINT('',(-1.005,4.3,4.5));
#7765=CARTESIAN_POINT('Origin',(0.,4.3,4.5));
#7766=CARTESIAN_POINT('',(-1.005,3.6,4.5));
#7767=CARTESIAN_POINT('Origin',(0.,3.6,4.5));
#7768=CARTESIAN_POINT('',(-2.34,4.3,4.5));
#7769=CARTESIAN_POINT('Origin',(0.,4.3,4.5));
#7770=CARTESIAN_POINT('',(-2.34,3.6,4.5));
#7771=CARTESIAN_POINT('',(-2.34,3.6,4.5));
#7772=CARTESIAN_POINT('Origin',(0.,3.6,4.5));
#7773=CARTESIAN_POINT('Origin',(0.,4.3,4.5));
#7774=CARTESIAN_POINT('Origin',(0.,3.6,4.5));
#7775=CARTESIAN_POINT('',(0.,0.,0.));
#7776=CARTESIAN_POINT('Origin',(0.,3.95,4.5));
#7777=CARTESIAN_POINT('',(-1.22464679914735E-16,3.95,5.5));
#7778=CARTESIAN_POINT('Origin',(-1.3164953090834E-16,3.95,5.575));
#7779=CARTESIAN_POINT('Origin',(0.,3.95,4.5));
#7780=CARTESIAN_POINT('',(0.,0.,0.));
#7781=CARTESIAN_POINT('Origin',(2.1,3.,4.5));
#7782=CARTESIAN_POINT('',(2.3165437617278,2.4,4.16950794260678));
#7783=CARTESIAN_POINT('',(2.1,2.4,4.16950794260678));
#7784=CARTESIAN_POINT('',(2.1,2.4,4.16950794260678));
#7785=CARTESIAN_POINT('',(2.3165437617278,3.6,4.16950794260679));
#7786=CARTESIAN_POINT('Ctrl Pts',(2.3165437617278,3.6,4.16950794260679));
#7787=CARTESIAN_POINT('Ctrl Pts',(2.30831151031136,3.56821604889379,4.11180498050191));
#7788=CARTESIAN_POINT('Ctrl Pts',(2.29860746123388,3.52826296991183,4.05952667968626));
#7789=CARTESIAN_POINT('Ctrl Pts',(2.27651111163957,3.42382665942891,3.95509036920334));
#7790=CARTESIAN_POINT('Ctrl Pts',(2.26271374962431,3.34714352725108,3.90246321020553));
#7791=CARTESIAN_POINT('Ctrl Pts',(2.24304290799559,3.17853989239017,3.83240559410195));
#7792=CARTESIAN_POINT('Ctrl Pts',(2.23749301674888,3.0865714655196,3.815));
#7793=CARTESIAN_POINT('Ctrl Pts',(2.23749301674888,3.,3.815));
#7794=CARTESIAN_POINT('Ctrl Pts',(2.23749301674888,2.9134285344804,3.815));
#7795=CARTESIAN_POINT('Ctrl Pts',(2.24304290799559,2.82146010760983,3.83240559410195));
#7796=CARTESIAN_POINT('Ctrl Pts',(2.26271374962431,2.65285647274892,3.90246321020553));
#7797=CARTESIAN_POINT('Ctrl Pts',(2.27651111163957,2.57617334057109,3.95509036920334));
#7798=CARTESIAN_POINT('Ctrl Pts',(2.29860746124079,2.47173703005551,4.05952667971892));
#7799=CARTESIAN_POINT('Ctrl Pts',(2.30831151030122,2.43178395114536,4.11180498043082));
#7800=CARTESIAN_POINT('Ctrl Pts',(2.3165437617278,2.4,4.16950794260678));
#7801=CARTESIAN_POINT('',(2.1,3.6,4.16950794260679));
#7802=CARTESIAN_POINT('',(2.1,3.6,4.16950794260679));
#7803=CARTESIAN_POINT('Origin',(2.1,3.,4.5));
#7804=CARTESIAN_POINT('Origin',(2.1,3.,4.5));
#7805=CARTESIAN_POINT('',(2.1,2.4,4.83049205739322));
#7806=CARTESIAN_POINT('',(2.3165437617278,2.4,4.83049205739322));
#7807=CARTESIAN_POINT('',(2.1,2.4,4.83049205739322));
#7808=CARTESIAN_POINT('',(2.1,3.6,4.83049205739321));
#7809=CARTESIAN_POINT('Origin',(2.1,3.,4.5));
#7810=CARTESIAN_POINT('',(2.3165437617278,3.6,4.83049205739322));
#7811=CARTESIAN_POINT('',(2.1,3.6,4.83049205739321));
#7812=CARTESIAN_POINT('Ctrl Pts',(2.3165437617278,2.4,4.83049205739322));
#7813=CARTESIAN_POINT('Ctrl Pts',(2.30831151030122,2.43178395114536,4.88819501956918));
#7814=CARTESIAN_POINT('Ctrl Pts',(2.29860746124079,2.47173703005551,4.94047332028108));
#7815=CARTESIAN_POINT('Ctrl Pts',(2.27651111163957,2.57617334057109,5.04490963079666));
#7816=CARTESIAN_POINT('Ctrl Pts',(2.26271374962431,2.65285647274892,5.09753678979447));
#7817=CARTESIAN_POINT('Ctrl Pts',(2.24304290799559,2.82146010760983,5.16759440589805));
#7818=CARTESIAN_POINT('Ctrl Pts',(2.23749301674888,2.9134285344804,5.185));
#7819=CARTESIAN_POINT('Ctrl Pts',(2.23749301674888,3.0865714655196,5.185));
#7820=CARTESIAN_POINT('Ctrl Pts',(2.24304290799559,3.17853989239017,5.16759440589805));
#7821=CARTESIAN_POINT('Ctrl Pts',(2.26271374962431,3.34714352725108,5.09753678979447));
#7822=CARTESIAN_POINT('Ctrl Pts',(2.27651111163957,3.42382665942891,5.04490963079666));
#7823=CARTESIAN_POINT('Ctrl Pts',(2.29860746124079,3.52826296994449,4.94047332028108));
#7824=CARTESIAN_POINT('Ctrl Pts',(2.30831151030122,3.56821604885464,4.88819501956918));
#7825=CARTESIAN_POINT('Ctrl Pts',(2.3165437617278,3.6,4.83049205739322));
#7826=CARTESIAN_POINT('Origin',(2.1,3.,4.5));
#7827=CARTESIAN_POINT('',(2.1,2.4,4.5));
#7828=CARTESIAN_POINT('',(2.1,3.6,4.5));
#7829=CARTESIAN_POINT('',(2.1,3.,4.96));
#7830=CARTESIAN_POINT('Origin',(2.1,3.,4.5));
#7831=CARTESIAN_POINT('Origin',(0.,3.6,4.5));
#7832=CARTESIAN_POINT('Origin',(0.,3.6,4.5));
#7833=CARTESIAN_POINT('',(-1.2,3.6,4.5));
#7834=CARTESIAN_POINT('Origin',(0.,3.6,4.5));
#7835=CARTESIAN_POINT('Origin',(0.,2.4,4.5));
#7836=CARTESIAN_POINT('Origin',(0.,2.4,4.5));
#7837=CARTESIAN_POINT('Origin',(0.,3.,4.5));
#7838=CARTESIAN_POINT('',(1.10833208019979,3.,4.04));
#7839=CARTESIAN_POINT('',(1.10833208019979,3.,4.96));
#7840=CARTESIAN_POINT('Ctrl Pts',(1.10833208019979,3.,4.04));
#7841=CARTESIAN_POINT('Ctrl Pts',(1.10833208019979,3.05843723698437,4.04));
#7842=CARTESIAN_POINT('Ctrl Pts',(1.11344185362589,3.12030150460074,4.05180175367034));
#7843=CARTESIAN_POINT('Ctrl Pts',(1.13126787543157,3.23342404964254,4.09891723731354));
#7844=CARTESIAN_POINT('Ctrl Pts',(1.14366370619736,3.2847433509607,4.13420511226908));
#7845=CARTESIAN_POINT('Ctrl Pts',(1.16647819892242,3.36576077881991,4.21522254012828));
#7846=CARTESIAN_POINT('Ctrl Pts',(1.17846362995473,3.40107463046863,4.26655493783234));
#7847=CARTESIAN_POINT('Ctrl Pts',(1.19532745919784,3.44820985363556,4.37972785158852));
#7848=CARTESIAN_POINT('Ctrl Pts',(1.2,3.46,4.44161194729012));
#7849=CARTESIAN_POINT('Ctrl Pts',(1.2,3.46,4.55838805270988));
#7850=CARTESIAN_POINT('Ctrl Pts',(1.19532745919784,3.44820985363556,4.62027214841148));
#7851=CARTESIAN_POINT('Ctrl Pts',(1.17846362995473,3.40107463046863,4.73344506216766));
#7852=CARTESIAN_POINT('Ctrl Pts',(1.16647819892242,3.36576077881991,4.78477745987172));
#7853=CARTESIAN_POINT('Ctrl Pts',(1.14366370619736,3.2847433509607,4.86579488773092));
#7854=CARTESIAN_POINT('Ctrl Pts',(1.13126787543157,3.23342404964254,4.90108276268646));
#7855=CARTESIAN_POINT('Ctrl Pts',(1.11344185362589,3.12030150460074,4.94819824632966));
#7856=CARTESIAN_POINT('Ctrl Pts',(1.10833208019979,3.05843723698437,4.96));
#7857=CARTESIAN_POINT('Ctrl Pts',(1.10833208019979,3.,4.96));
#7858=CARTESIAN_POINT('Ctrl Pts',(1.10833208019979,3.,4.96));
#7859=CARTESIAN_POINT('Ctrl Pts',(1.10833208019979,2.94156276301563,4.96));
#7860=CARTESIAN_POINT('Ctrl Pts',(1.11344185362589,2.87969849539926,4.94819824632966));
#7861=CARTESIAN_POINT('Ctrl Pts',(1.13126787543157,2.76657595035746,4.90108276268646));
#7862=CARTESIAN_POINT('Ctrl Pts',(1.14366370619736,2.7152566490393,4.86579488773092));
#7863=CARTESIAN_POINT('Ctrl Pts',(1.16647819892242,2.63423922118009,4.78477745987172));
#7864=CARTESIAN_POINT('Ctrl Pts',(1.17846362995473,2.59892536953137,4.73344506216766));
#7865=CARTESIAN_POINT('Ctrl Pts',(1.19532745919784,2.55179014636444,4.62027214841148));
#7866=CARTESIAN_POINT('Ctrl Pts',(1.2,2.54,4.55838805270988));
#7867=CARTESIAN_POINT('Ctrl Pts',(1.2,2.54,4.44161194729012));
#7868=CARTESIAN_POINT('Ctrl Pts',(1.19532745919784,2.55179014636444,4.37972785158852));
#7869=CARTESIAN_POINT('Ctrl Pts',(1.17846362995473,2.59892536953137,4.26655493783234));
#7870=CARTESIAN_POINT('Ctrl Pts',(1.16647819892242,2.63423922118009,4.21522254012828));
#7871=CARTESIAN_POINT('Ctrl Pts',(1.14366370619736,2.7152566490393,4.13420511226908));
#7872=CARTESIAN_POINT('Ctrl Pts',(1.13126787543157,2.76657595035746,4.09891723731354));
#7873=CARTESIAN_POINT('Ctrl Pts',(1.11344185362589,2.87969849539925,4.05180175367034));
#7874=CARTESIAN_POINT('Ctrl Pts',(1.10833208019979,2.94156276301563,4.04));
#7875=CARTESIAN_POINT('Ctrl Pts',(1.10833208019979,3.,4.04));
#7876=CARTESIAN_POINT('',(0.,3.,4.96));
#7877=CARTESIAN_POINT('Origin',(0.,2.4,4.5));
#7878=CARTESIAN_POINT('',(-1.2,2.4,4.5));
#7879=CARTESIAN_POINT('',(-1.2,2.4,4.5));
#7880=CARTESIAN_POINT('Origin',(0.,2.4,4.5));
#7881=CARTESIAN_POINT('Origin',(0.,2.4,4.5));
#7882=CARTESIAN_POINT('',(0.,0.,0.));
#7883=CARTESIAN_POINT('Origin',(-2.8,-0.5,4.5));
#7884=CARTESIAN_POINT('',(-3.025,-0.4,4.5));
#7885=CARTESIAN_POINT('Origin',(-2.8,-0.4,4.5));
#7886=CARTESIAN_POINT('',(-3.025,0.,4.5));
#7887=CARTESIAN_POINT('',(-3.025,-0.5,4.5));
#7888=CARTESIAN_POINT('Origin',(-2.8,0.,4.5));
#7889=CARTESIAN_POINT('Origin',(1.71450551880629E-16,-0.5,7.3));
#7890=CARTESIAN_POINT('',(-0.225,-0.4,7.3));
#7891=CARTESIAN_POINT('Origin',(1.71450551880629E-16,-0.4,7.3));
#7892=CARTESIAN_POINT('',(-0.225,0.,7.3));
#7893=CARTESIAN_POINT('',(-0.225,-0.5,7.3));
#7894=CARTESIAN_POINT('Origin',(1.71450551880629E-16,0.,7.3));
#7895=CARTESIAN_POINT('Origin',(2.8,-0.5,4.5));
#7896=CARTESIAN_POINT('',(2.575,-0.4,4.5));
#7897=CARTESIAN_POINT('Origin',(2.8,-0.4,4.5));
#7898=CARTESIAN_POINT('',(2.575,0.,4.5));
#7899=CARTESIAN_POINT('',(2.575,-0.5,4.5));
#7900=CARTESIAN_POINT('Origin',(2.8,0.,4.5));
#7901=CARTESIAN_POINT('Origin',(-5.14351655641888E-16,-0.5,1.7));
#7902=CARTESIAN_POINT('',(-0.225000000000001,-0.4,1.7));
#7903=CARTESIAN_POINT('Origin',(-5.14351655641888E-16,-0.4,1.7));
#7904=CARTESIAN_POINT('',(-0.225000000000001,0.,1.7));
#7905=CARTESIAN_POINT('',(-0.225000000000001,-0.5,1.7));
#7906=CARTESIAN_POINT('Origin',(-5.14351655641888E-16,0.,1.7));
#7907=CARTESIAN_POINT('Origin',(0.,0.,4.5));
#7908=CARTESIAN_POINT('',(-2.34,0.3,4.5));
#7909=CARTESIAN_POINT('Origin',(0.,0.3,4.5));
#7910=CARTESIAN_POINT('',(-2.34,0.,4.5));
#7911=CARTESIAN_POINT('',(-2.34,0.,4.5));
#7912=CARTESIAN_POINT('Origin',(0.,0.,4.5));
#7913=CARTESIAN_POINT('Origin',(0.,0.3,4.5));
#7914=CARTESIAN_POINT('',(-1.8,0.3,4.5));
#7915=CARTESIAN_POINT('Origin',(0.,0.3,4.5));
#7916=CARTESIAN_POINT('Origin',(0.,-0.4,4.5));
#7917=CARTESIAN_POINT('',(-1.8,-0.4,4.5));
#7918=CARTESIAN_POINT('',(-1.8,-0.4,4.5));
#7919=CARTESIAN_POINT('Origin',(0.,-0.4,4.5));
#7920=CARTESIAN_POINT('Origin',(0.,-0.4,4.5));
#7921=CARTESIAN_POINT('',(-3.5,0.,4.5));
#7922=CARTESIAN_POINT('Origin',(0.,0.,4.5));
#7923=CARTESIAN_POINT('',(-3.5,-0.4,4.5));
#7924=CARTESIAN_POINT('',(-3.5,-0.4,4.5));
#7925=CARTESIAN_POINT('Origin',(0.,-0.4,4.5));
#7926=CARTESIAN_POINT('Origin',(0.,0.,4.5));
#7927=CARTESIAN_POINT('Origin',(0.,-0.4,4.5));
#7928=CARTESIAN_POINT('',(0.,0.,0.));
#7929=CARTESIAN_POINT('Origin',(-2.8,5.9,4.5));
#7930=CARTESIAN_POINT('',(-3.025,6.,4.5));
#7931=CARTESIAN_POINT('Origin',(-2.8,6.,4.5));
#7932=CARTESIAN_POINT('',(-3.025,6.4,4.5));
#7933=CARTESIAN_POINT('',(-3.025,5.9,4.5));
#7934=CARTESIAN_POINT('Origin',(-2.8,6.4,4.5));
#7935=CARTESIAN_POINT('Origin',(1.71450551880629E-16,5.9,7.3));
#7936=CARTESIAN_POINT('',(-0.225,6.,7.3));
#7937=CARTESIAN_POINT('Origin',(1.71450551880629E-16,6.,7.3));
#7938=CARTESIAN_POINT('',(-0.225,6.4,7.3));
#7939=CARTESIAN_POINT('',(-0.225,5.9,7.3));
#7940=CARTESIAN_POINT('Origin',(1.71450551880629E-16,6.4,7.3));
#7941=CARTESIAN_POINT('Origin',(2.8,5.9,4.5));
#7942=CARTESIAN_POINT('',(2.575,6.,4.5));
#7943=CARTESIAN_POINT('Origin',(2.8,6.,4.5));
#7944=CARTESIAN_POINT('',(2.575,6.4,4.5));
#7945=CARTESIAN_POINT('',(2.575,5.9,4.5));
#7946=CARTESIAN_POINT('Origin',(2.8,6.4,4.5));
#7947=CARTESIAN_POINT('Origin',(-5.14351655641888E-16,5.9,1.7));
#7948=CARTESIAN_POINT('',(-0.225000000000001,6.,1.7));
#7949=CARTESIAN_POINT('Origin',(-5.14351655641888E-16,6.,1.7));
#7950=CARTESIAN_POINT('',(-0.225000000000001,6.4,1.7));
#7951=CARTESIAN_POINT('',(-0.225000000000001,5.9,1.7));
#7952=CARTESIAN_POINT('Origin',(-5.14351655641888E-16,6.4,1.7));
#7953=CARTESIAN_POINT('Origin',(0.,5.7,4.5));
#7954=CARTESIAN_POINT('',(-2.34,6.,4.5));
#7955=CARTESIAN_POINT('Origin',(0.,6.,4.5));
#7956=CARTESIAN_POINT('',(-2.34,5.7,4.5));
#7957=CARTESIAN_POINT('',(-2.34,5.7,4.5));
#7958=CARTESIAN_POINT('Origin',(0.,5.7,4.5));
#7959=CARTESIAN_POINT('Origin',(0.,5.7,4.5));
#7960=CARTESIAN_POINT('',(-1.8,5.7,4.5));
#7961=CARTESIAN_POINT('Origin',(0.,5.7,4.5));
#7962=CARTESIAN_POINT('Origin',(0.,6.,4.5));
#7963=CARTESIAN_POINT('',(-1.8,6.4,4.5));
#7964=CARTESIAN_POINT('Origin',(0.,6.4,4.5));
#7965=CARTESIAN_POINT('',(-1.8,6.,4.5));
#7966=CARTESIAN_POINT('Origin',(0.,6.,4.5));
#7967=CARTESIAN_POINT('',(-3.5,6.4,4.5));
#7968=CARTESIAN_POINT('Origin',(0.,6.4,4.5));
#7969=CARTESIAN_POINT('',(-3.5,6.,4.5));
#7970=CARTESIAN_POINT('',(-3.5,6.,4.5));
#7971=CARTESIAN_POINT('Origin',(0.,6.,4.5));
#7972=CARTESIAN_POINT('Origin',(0.,6.4,4.5));
#7973=CARTESIAN_POINT('Origin',(0.,6.,4.5));
#7974=CARTESIAN_POINT('',(0.,0.,0.));
#7975=CARTESIAN_POINT('Origin',(5.5,0.,-0.3));
#7976=CARTESIAN_POINT('',(5.5,0.,-0.3));
#7977=CARTESIAN_POINT('',(-5.5,0.,-0.3));
#7978=CARTESIAN_POINT('',(5.5,0.,-0.3));
#7979=CARTESIAN_POINT('',(-5.5,0.,0.));
#7980=CARTESIAN_POINT('',(-5.5,0.,-0.3));
#7981=CARTESIAN_POINT('',(5.5,0.,0.));
#7982=CARTESIAN_POINT('',(5.5,0.,0.));
#7983=CARTESIAN_POINT('',(5.5,0.,-0.3));
#7984=CARTESIAN_POINT('Origin',(5.5,-1.,-0.3));
#7985=CARTESIAN_POINT('',(5.5,-1.,-0.3));
#7986=CARTESIAN_POINT('',(5.5,-1.,-0.3));
#7987=CARTESIAN_POINT('',(5.5,-1.,0.));
#7988=CARTESIAN_POINT('',(5.5,-1.,0.));
#7989=CARTESIAN_POINT('',(5.5,-1.,-0.3));
#7990=CARTESIAN_POINT('Origin',(-5.5,-1.,-0.3));
#7991=CARTESIAN_POINT('',(-5.5,-1.,-0.3));
#7992=CARTESIAN_POINT('',(-5.5,-1.,-0.3));
#7993=CARTESIAN_POINT('',(-5.5,-1.,0.));
#7994=CARTESIAN_POINT('',(-5.5,-1.,0.));
#7995=CARTESIAN_POINT('',(-5.5,-1.,-0.3));
#7996=CARTESIAN_POINT('Origin',(-5.5,0.,-0.3));
#7997=CARTESIAN_POINT('',(-5.5,0.,-0.3));
#7998=CARTESIAN_POINT('',(-5.5,0.,0.));
#7999=CARTESIAN_POINT('Origin',(0.,-0.5,0.));
#8000=CARTESIAN_POINT('Origin',(0.,-0.5,-0.3));
#8001=CARTESIAN_POINT('',(0.,0.,0.));
#8002=CARTESIAN_POINT('Origin',(5.5,7.,-0.3));
#8003=CARTESIAN_POINT('',(5.5,7.,-0.3));
#8004=CARTESIAN_POINT('',(-5.5,7.,-0.3));
#8005=CARTESIAN_POINT('',(5.5,7.,-0.3));
#8006=CARTESIAN_POINT('',(-5.5,7.,0.));
#8007=CARTESIAN_POINT('',(-5.5,7.,-0.3));
#8008=CARTESIAN_POINT('',(5.5,7.,0.));
#8009=CARTESIAN_POINT('',(5.5,7.,0.));
#8010=CARTESIAN_POINT('',(5.5,7.,-0.3));
#8011=CARTESIAN_POINT('Origin',(5.5,6.,-0.3));
#8012=CARTESIAN_POINT('',(5.5,6.,-0.3));
#8013=CARTESIAN_POINT('',(5.5,6.,-0.3));
#8014=CARTESIAN_POINT('',(5.5,6.,0.));
#8015=CARTESIAN_POINT('',(5.5,6.,0.));
#8016=CARTESIAN_POINT('',(5.5,6.,-0.3));
#8017=CARTESIAN_POINT('Origin',(-5.5,6.,-0.3));
#8018=CARTESIAN_POINT('',(-5.5,6.,-0.3));
#8019=CARTESIAN_POINT('',(-5.5,6.,-0.3));
#8020=CARTESIAN_POINT('',(-5.5,6.,0.));
#8021=CARTESIAN_POINT('',(-5.5,6.,0.));
#8022=CARTESIAN_POINT('',(-5.5,6.,-0.3));
#8023=CARTESIAN_POINT('Origin',(-5.5,7.,-0.3));
#8024=CARTESIAN_POINT('',(-5.5,7.,-0.3));
#8025=CARTESIAN_POINT('',(-5.5,7.,0.));
#8026=CARTESIAN_POINT('Origin',(0.,6.5,0.));
#8027=CARTESIAN_POINT('Origin',(0.,6.5,-0.3));
#8028=CARTESIAN_POINT('',(0.,0.,0.));
#8029=CARTESIAN_POINT('',(0.,0.,0.));
#8030=CARTESIAN_POINT('Origin',(0.,0.,0.));
#8031=CARTESIAN_POINT('',(-1.63531,-0.410863395882378,-2.00267715711366E-16));
#8032=CARTESIAN_POINT('',(-2.00267715711366E-16,-0.410863395882378,1.63531));
#8033=CARTESIAN_POINT('Origin',(0.,-0.410863395882378,0.));
#8034=CARTESIAN_POINT('Origin',(0.,-0.410863395882378,0.));
#8035=CARTESIAN_POINT('',(-2.00267715711366E-16,0.410863395882378,1.63531));
#8036=CARTESIAN_POINT('Origin',(-2.05128338857182E-16,0.,1.675));
#8037=CARTESIAN_POINT('',(-1.63531,0.410863395882378,2.00267715711366E-16));
#8038=CARTESIAN_POINT('Origin',(0.,0.410863395882378,0.));
#8039=CARTESIAN_POINT('Origin',(0.,0.410863395882378,0.));
#8040=CARTESIAN_POINT('Origin',(0.,0.,0.));
#8041=CARTESIAN_POINT('',(-1.63531,0.7,-2.00267715711366E-16));
#8042=CARTESIAN_POINT('',(-1.63531,0.,-2.00267715711366E-16));
#8043=CARTESIAN_POINT('Origin',(0.,0.7,0.));
#8044=CARTESIAN_POINT('Origin',(0.,0.,0.));
#8045=CARTESIAN_POINT('',(-1.,-0.6,-1.22464679914735E-16));
#8046=CARTESIAN_POINT('Origin',(0.,-0.6,0.));
#8047=CARTESIAN_POINT('',(-1.,0.6,-1.22464679914735E-16));
#8048=CARTESIAN_POINT('',(-1.,0.,-1.22464679914735E-16));
#8049=CARTESIAN_POINT('Origin',(0.,0.6,0.));
#8050=CARTESIAN_POINT('Origin',(0.,0.65,0.));
#8051=CARTESIAN_POINT('',(-1.1,0.7,-1.34711147906209E-16));
#8052=CARTESIAN_POINT('',(-1.05,0.65,-1.28587913910472E-16));
#8053=CARTESIAN_POINT('Origin',(0.,0.7,0.));
#8054=CARTESIAN_POINT('Origin',(1.63531,0.7,0.));
#8055=CARTESIAN_POINT('Origin',(0.,0.,0.));
#8056=CARTESIAN_POINT('',(-1.63531,-0.7,-2.00267715711366E-16));
#8057=CARTESIAN_POINT('Origin',(0.,-0.7,0.));
#8058=CARTESIAN_POINT('',(-1.63531,0.,-2.00267715711366E-16));
#8059=CARTESIAN_POINT('Origin',(1.1,-0.7,0.));
#8060=CARTESIAN_POINT('',(-1.1,-0.7,-1.34711147906209E-16));
#8061=CARTESIAN_POINT('Origin',(0.,-0.7,0.));
#8062=CARTESIAN_POINT('Origin',(0.,-0.65,0.));
#8063=CARTESIAN_POINT('',(-1.05,-0.65,-1.28587913910472E-16));
#8064=CARTESIAN_POINT('',(0.,0.,0.));
#8065=CARTESIAN_POINT('Origin',(0.,0.,0.));
#8066=CARTESIAN_POINT('',(-1.71469,0.410863395882378,-2.09988962002998E-16));
#8067=CARTESIAN_POINT('',(-2.09988962002998E-16,0.410863395882378,1.71469));
#8068=CARTESIAN_POINT('Origin',(0.,0.410863395882378,0.));
#8069=CARTESIAN_POINT('Origin',(0.,0.410863395882378,0.));
#8070=CARTESIAN_POINT('',(-2.09988962002998E-16,-0.410863395882378,1.71469));
#8071=CARTESIAN_POINT('Origin',(-2.05128338857182E-16,0.,1.675));
#8072=CARTESIAN_POINT('',(-1.71469,-0.410863395882378,2.09988962002998E-16));
#8073=CARTESIAN_POINT('Origin',(0.,-0.410863395882378,0.));
#8074=CARTESIAN_POINT('Origin',(0.,-0.410863395882378,0.));
#8075=CARTESIAN_POINT('Origin',(0.,0.,0.));
#8076=CARTESIAN_POINT('',(-1.71469,-0.7,-2.09988962002998E-16));
#8077=CARTESIAN_POINT('Origin',(0.,-0.7,0.));
#8078=CARTESIAN_POINT('',(-1.71469,0.,-2.09988962002998E-16));
#8079=CARTESIAN_POINT('Origin',(2.25,0.7,0.));
#8080=CARTESIAN_POINT('',(-2.25,0.7,-2.75545529808154E-16));
#8081=CARTESIAN_POINT('Origin',(0.,0.7,0.));
#8082=CARTESIAN_POINT('',(-1.71469,0.7,-2.09988962002998E-16));
#8083=CARTESIAN_POINT('Origin',(0.,0.7,0.));
#8084=CARTESIAN_POINT('Origin',(0.,0.65,0.));
#8085=CARTESIAN_POINT('',(-2.35,0.6,-2.87791997799628E-16));
#8086=CARTESIAN_POINT('Origin',(0.,0.6,0.));
#8087=CARTESIAN_POINT('',(-2.3,0.65,-2.81668763803891E-16));
#8088=CARTESIAN_POINT('Origin',(0.,0.,0.));
#8089=CARTESIAN_POINT('',(-2.35,-0.6,-2.87791997799628E-16));
#8090=CARTESIAN_POINT('Origin',(0.,-0.6,0.));
#8091=CARTESIAN_POINT('',(-2.35,0.,-2.87791997799628E-16));
#8092=CARTESIAN_POINT('Origin',(0.,-0.65,0.));
#8093=CARTESIAN_POINT('',(-2.25,-0.7,-2.75545529808154E-16));
#8094=CARTESIAN_POINT('Origin',(0.,-0.7,0.));
#8095=CARTESIAN_POINT('',(-2.3,-0.65,-2.81668763803891E-16));
#8096=CARTESIAN_POINT('Origin',(1.71469,-0.7,0.));
#8097=CARTESIAN_POINT('Origin',(0.,0.,0.));
#8098=CARTESIAN_POINT('',(-1.71469,0.,-2.09988962002998E-16));
#8099=CARTESIAN_POINT('',(0.,0.,0.));
#8100=CARTESIAN_POINT('Origin',(1.675,0.,0.));
#8101=CARTESIAN_POINT('',(1.675,-2.97627328869245E-33,0.3969));
#8102=CARTESIAN_POINT('',(1.675,-2.97627328869245E-33,-0.3969));
#8103=CARTESIAN_POINT('Origin',(1.675,0.,0.));
#8104=CARTESIAN_POINT('Origin',(1.18440385848747,0.,-1.18440385848747));
#8105=CARTESIAN_POINT('',(1.46505453994041,3.1867025333467E-33,-0.903753177034526));
#8106=CARTESIAN_POINT('',(0.903753177034527,-9.13924911073161E-33,-1.46505453994041));
#8107=CARTESIAN_POINT('Origin',(1.18440385848747,0.,-1.18440385848747));
#8108=CARTESIAN_POINT('Origin',(1.02564169428591E-16,0.,-1.675));
#8109=CARTESIAN_POINT('',(0.3969,-2.97627328869246E-33,-1.675));
#8110=CARTESIAN_POINT('',(-0.3969,-2.97627328869245E-33,-1.675));
#8111=CARTESIAN_POINT('Origin',(1.02564169428591E-16,0.,-1.675));
#8112=CARTESIAN_POINT('Origin',(-1.18440385848747,0.,-1.18440385848747));
#8113=CARTESIAN_POINT('',(-0.903753177034526,3.1867025333467E-33,-1.46505453994041));
#8114=CARTESIAN_POINT('',(-1.46505453994041,-9.13924911073161E-33,-0.903753177034527));
#8115=CARTESIAN_POINT('Origin',(-1.18440385848747,0.,-1.18440385848747));
#8116=CARTESIAN_POINT('Origin',(-1.675,0.,-2.05128338857182E-16));
#8117=CARTESIAN_POINT('',(-1.675,-2.97627328869246E-33,-0.3969));
#8118=CARTESIAN_POINT('',(-1.675,-2.97627328869245E-33,0.3969));
#8119=CARTESIAN_POINT('Origin',(-1.675,0.,-2.05128338857182E-16));
#8120=CARTESIAN_POINT('Origin',(-1.18440385848747,0.,1.18440385848747));
#8121=CARTESIAN_POINT('',(-1.46505453994041,6.26819044436628E-33,0.903753177034526));
#8122=CARTESIAN_POINT('',(-0.903753177034527,-1.22207370217512E-32,1.46505453994041));
#8123=CARTESIAN_POINT('Origin',(-1.18440385848747,0.,1.18440385848747));
#8124=CARTESIAN_POINT('Origin',(-3.07692508285772E-16,0.,1.675));
#8125=CARTESIAN_POINT('',(-0.3969,-2.97627328869246E-33,1.675));
#8126=CARTESIAN_POINT('',(0.396899999999999,-2.97627328869245E-33,1.675));
#8127=CARTESIAN_POINT('Origin',(-3.07692508285772E-16,0.,1.675));
#8128=CARTESIAN_POINT('Origin',(1.18440385848747,0.,1.18440385848747));
#8129=CARTESIAN_POINT('',(0.903753177034526,9.34967835538585E-33,1.46505453994041));
#8130=CARTESIAN_POINT('',(1.46505453994041,-1.53022249327708E-32,0.903753177034527));
#8131=CARTESIAN_POINT('Origin',(1.18440385848747,0.,1.18440385848747));
#8132=CARTESIAN_POINT('',(0.,0.,0.));
#8133=CARTESIAN_POINT('Origin',(1.18440385848747,0.,1.18440385848747));
#8134=CARTESIAN_POINT('',(0.846804978391753,-0.07938,1.40825612658882));
#8135=CARTESIAN_POINT('',(1.40825612658882,-0.07938,0.846804978391754));
#8136=CARTESIAN_POINT('Ctrl Pts',(0.846804978391752,-0.0793800000000001,
1.40825612658882));
#8137=CARTESIAN_POINT('Ctrl Pts',(0.854205272175554,-0.123401821157026,
1.40380622184538));
#8138=CARTESIAN_POINT('Ctrl Pts',(0.867957148219441,-0.166543350814306,
1.39550172959303));
#8139=CARTESIAN_POINT('Ctrl Pts',(0.902193646979982,-0.237231147975234,
1.3735491215176));
#8140=CARTESIAN_POINT('Ctrl Pts',(0.920778333482564,-0.266264900654909,
1.36127834356734));
#8141=CARTESIAN_POINT('Ctrl Pts',(0.962485392528369,-0.317195968905306,
1.33211611256184));
#8142=CARTESIAN_POINT('Ctrl Pts',(0.985600426557816,-0.33909093068465,1.31521005565926));
#8143=CARTESIAN_POINT('Ctrl Pts',(1.03253285680459,-0.373586846396559,1.27866649102984));
#8144=CARTESIAN_POINT('Ctrl Pts',(1.05871835910697,-0.388086240756494,1.25722555095714));
#8145=CARTESIAN_POINT('Ctrl Pts',(1.11153475808518,-0.407068917407805,1.2107812086231));
#8146=CARTESIAN_POINT('Ctrl Pts',(1.13814686046673,-0.411552957311693,1.18575674747573));
#8147=CARTESIAN_POINT('Ctrl Pts',(1.18575674747573,-0.411552957311693,1.13814686046673));
#8148=CARTESIAN_POINT('Ctrl Pts',(1.2107812086231,-0.407068917407805,1.11153475808518));
#8149=CARTESIAN_POINT('Ctrl Pts',(1.25722555095713,-0.388086240756494,1.05871835910697));
#8150=CARTESIAN_POINT('Ctrl Pts',(1.27866649102984,-0.373586846396559,1.03253285680459));
#8151=CARTESIAN_POINT('Ctrl Pts',(1.31521005565926,-0.33909093068465,0.985600426557816));
#8152=CARTESIAN_POINT('Ctrl Pts',(1.33211611256184,-0.317195968905306,0.962485392528369));
#8153=CARTESIAN_POINT('Ctrl Pts',(1.36127834356734,-0.266264900654909,0.920778333482565));
#8154=CARTESIAN_POINT('Ctrl Pts',(1.3735491215176,-0.237231147975234,0.902193646979983));
#8155=CARTESIAN_POINT('Ctrl Pts',(1.39550172959303,-0.166543350814306,0.867957148219442));
#8156=CARTESIAN_POINT('Ctrl Pts',(1.40380622184538,-0.123401821157026,0.854205272175555));
#8157=CARTESIAN_POINT('Ctrl Pts',(1.40825612658882,-0.0793800000000001,
0.846804978391753));
#8158=CARTESIAN_POINT('',(0.886256117232623,-0.07938,1.45861320581289));
#8159=CARTESIAN_POINT('Origin',(1.18440385848747,-0.07938,1.18440385848747));
#8160=CARTESIAN_POINT('',(1.45861320581289,-0.07938,0.886256117232624));
#8161=CARTESIAN_POINT('Ctrl Pts',(1.45861320581289,-0.0793800000000001,
0.886256117232623));
#8162=CARTESIAN_POINT('Ctrl Pts',(1.45630208793976,-0.101649918886749,0.890059788636852));
#8163=CARTESIAN_POINT('Ctrl Pts',(1.45296717977858,-0.123823518623746,0.895520212222107));
#8164=CARTESIAN_POINT('Ctrl Pts',(1.43904931717599,-0.192480977588836,0.917859913453975));
#8165=CARTESIAN_POINT('Ctrl Pts',(1.4243271592157,-0.236152929235938,0.940896403863072));
#8166=CARTESIAN_POINT('Ctrl Pts',(1.39055359345152,-0.303141259068212,0.990027513266106));
#8167=CARTESIAN_POINT('Ctrl Pts',(1.36743459453896,-0.335108247315849,1.02199477007745));
#8168=CARTESIAN_POINT('Ctrl Pts',(1.32643091652006,-0.373243761060364,1.07446535104584));
#8169=CARTESIAN_POINT('Ctrl Pts',(1.30441816675528,-0.387888272594439,1.10126842659597));
#8170=CARTESIAN_POINT('Ctrl Pts',(1.25681160160691,-0.407041111792943,1.15530234155453));
#8171=CARTESIAN_POINT('Ctrl Pts',(1.23119764287622,-0.411552957311693,1.18251418313119));
#8172=CARTESIAN_POINT('Ctrl Pts',(1.18251418313119,-0.411552957311693,1.23119764287622));
#8173=CARTESIAN_POINT('Ctrl Pts',(1.15530234155453,-0.407041111792943,1.25681160160691));
#8174=CARTESIAN_POINT('Ctrl Pts',(1.10126842659597,-0.387888272594439,1.30441816675528));
#8175=CARTESIAN_POINT('Ctrl Pts',(1.07446535104584,-0.373243761060364,1.32643091652006));
#8176=CARTESIAN_POINT('Ctrl Pts',(1.02199477007745,-0.335108247315848,1.36743459453896));
#8177=CARTESIAN_POINT('Ctrl Pts',(0.990027513266105,-0.303141259068211,
1.39055359345152));
#8178=CARTESIAN_POINT('Ctrl Pts',(0.940896403863071,-0.236152929235937,
1.42432715921571));
#8179=CARTESIAN_POINT('Ctrl Pts',(0.917859913453974,-0.192480977588835,
1.43904931717599));
#8180=CARTESIAN_POINT('Ctrl Pts',(0.895520212222106,-0.123823518623745,
1.45296717977858));
#8181=CARTESIAN_POINT('Ctrl Pts',(0.890059788636851,-0.101649918886749,
1.45630208793976));
#8182=CARTESIAN_POINT('Ctrl Pts',(0.886256117232622,-0.0793800000000001,
1.45861320581289));
#8183=CARTESIAN_POINT('Origin',(1.18440385848747,-0.07938,1.18440385848747));
#8184=CARTESIAN_POINT('Origin',(0.,-0.27783,0.));
#8185=CARTESIAN_POINT('',(0.404717578595295,-0.07938,1.65807299932179));
#8186=CARTESIAN_POINT('Origin',(0.,-0.07938,0.));
#8187=CARTESIAN_POINT('',(-0.404717578595296,-0.07938,1.65807299932179));
#8188=CARTESIAN_POINT('Ctrl Pts',(0.404717578595296,-0.0793800000000001,
1.65807299932179));
#8189=CARTESIAN_POINT('Ctrl Pts',(0.400393769631747,-0.101649918886749,
1.65912839404491));
#8190=CARTESIAN_POINT('Ctrl Pts',(0.394174530911058,-0.123823518623745,
1.66063136041479));
#8191=CARTESIAN_POINT('Ctrl Pts',(0.368536561654407,-0.192480977588835,
1.66658649961961));
#8192=CARTESIAN_POINT('Ctrl Pts',(0.341837165343982,-0.236152929235937,
1.67246562047521));
#8193=CARTESIAN_POINT('Ctrl Pts',(0.283214707341173,-0.303141259068211,
1.68332504372461));
#8194=CARTESIAN_POINT('Ctrl Pts',(0.244262842368623,-0.335108247315849,
1.68958170688653));
#8195=CARTESIAN_POINT('Ctrl Pts',(0.178166559972324,-0.373243761060364,
1.69769003172132));
#8196=CARTESIAN_POINT('Ctrl Pts',(0.143648558862931,-0.387888272594439,
1.70107730356824));
#8197=CARTESIAN_POINT('Ctrl Pts',(0.0717778861362652,-0.407041111792943,
1.70562212620408));
#8198=CARTESIAN_POINT('Ctrl Pts',(0.0344244045173309,-0.411552957311693,
1.706752));
#8199=CARTESIAN_POINT('Ctrl Pts',(-0.0344244045173315,-0.411552957311693,
1.706752));
#8200=CARTESIAN_POINT('Ctrl Pts',(-0.0717778861362658,-0.407041111792943,
1.70562212620408));
#8201=CARTESIAN_POINT('Ctrl Pts',(-0.143648558862932,-0.387888272594439,
1.70107730356824));
#8202=CARTESIAN_POINT('Ctrl Pts',(-0.178166559972325,-0.373243761060364,
1.69769003172132));
#8203=CARTESIAN_POINT('Ctrl Pts',(-0.244262842368624,-0.335108247315849,
1.68958170688653));
#8204=CARTESIAN_POINT('Ctrl Pts',(-0.283214707341173,-0.303141259068212,
1.68332504372461));
#8205=CARTESIAN_POINT('Ctrl Pts',(-0.341837165343982,-0.236152929235937,
1.67246562047521));
#8206=CARTESIAN_POINT('Ctrl Pts',(-0.368536561654408,-0.192480977588835,
1.66658649961961));
#8207=CARTESIAN_POINT('Ctrl Pts',(-0.394174530911059,-0.123823518623745,
1.66063136041479));
#8208=CARTESIAN_POINT('Ctrl Pts',(-0.400393769631748,-0.101649918886749,
1.65912839404491));
#8209=CARTESIAN_POINT('Ctrl Pts',(-0.404717578595297,-0.0793800000000001,
1.65807299932179));
#8210=CARTESIAN_POINT('',(-0.886256117232624,-0.07938,1.45861320581289));
#8211=CARTESIAN_POINT('Origin',(0.,-0.07938,0.));
#8212=CARTESIAN_POINT('',(-1.45861320581289,-0.07938,0.886256117232623));
#8213=CARTESIAN_POINT('Ctrl Pts',(-0.886256117232623,-0.0793800000000001,
1.45861320581289));
#8214=CARTESIAN_POINT('Ctrl Pts',(-0.890059788636852,-0.101649918886749,
1.45630208793976));
#8215=CARTESIAN_POINT('Ctrl Pts',(-0.895520212222106,-0.123823518623745,
1.45296717977858));
#8216=CARTESIAN_POINT('Ctrl Pts',(-0.917859913453974,-0.192480977588835,
1.43904931717599));
#8217=CARTESIAN_POINT('Ctrl Pts',(-0.940896403863071,-0.236152929235937,
1.4243271592157));
#8218=CARTESIAN_POINT('Ctrl Pts',(-0.990027513266105,-0.303141259068211,
1.39055359345152));
#8219=CARTESIAN_POINT('Ctrl Pts',(-1.02199477007745,-0.335108247315848,
1.36743459453896));
#8220=CARTESIAN_POINT('Ctrl Pts',(-1.07446535104584,-0.373243761060364,
1.32643091652006));
#8221=CARTESIAN_POINT('Ctrl Pts',(-1.10126842659597,-0.387888272594439,
1.30441816675528));
#8222=CARTESIAN_POINT('Ctrl Pts',(-1.15530234155453,-0.407041111792943,
1.25681160160691));
#8223=CARTESIAN_POINT('Ctrl Pts',(-1.18251418313119,-0.411552957311693,
1.23119764287622));
#8224=CARTESIAN_POINT('Ctrl Pts',(-1.23119764287622,-0.411552957311693,
1.18251418313119));
#8225=CARTESIAN_POINT('Ctrl Pts',(-1.25681160160691,-0.407041111792943,
1.15530234155453));
#8226=CARTESIAN_POINT('Ctrl Pts',(-1.30441816675528,-0.387888272594439,
1.10126842659597));
#8227=CARTESIAN_POINT('Ctrl Pts',(-1.32643091652006,-0.373243761060365,
1.07446535104584));
#8228=CARTESIAN_POINT('Ctrl Pts',(-1.36743459453896,-0.335108247315849,
1.02199477007745));
#8229=CARTESIAN_POINT('Ctrl Pts',(-1.39055359345152,-0.303141259068212,
0.990027513266106));
#8230=CARTESIAN_POINT('Ctrl Pts',(-1.4243271592157,-0.236152929235938,0.940896403863071));
#8231=CARTESIAN_POINT('Ctrl Pts',(-1.43904931717599,-0.192480977588836,
0.917859913453974));
#8232=CARTESIAN_POINT('Ctrl Pts',(-1.45296717977858,-0.123823518623746,
0.895520212222106));
#8233=CARTESIAN_POINT('Ctrl Pts',(-1.45630208793976,-0.101649918886749,
0.890059788636852));
#8234=CARTESIAN_POINT('Ctrl Pts',(-1.45861320581289,-0.0793800000000001,
0.886256117232623));
#8235=CARTESIAN_POINT('',(-1.65807299932179,-0.07938,0.404717578595295));
#8236=CARTESIAN_POINT('Origin',(0.,-0.07938,0.));
#8237=CARTESIAN_POINT('',(-1.706752,-0.411552957311693,2.08591827245526E-16));
#8238=CARTESIAN_POINT('Ctrl Pts',(-1.65807299932179,-0.0793800000000001,
0.404717578595296));
#8239=CARTESIAN_POINT('Ctrl Pts',(-1.65912839404491,-0.101649918886749,
0.400393769631747));
#8240=CARTESIAN_POINT('Ctrl Pts',(-1.66063136041479,-0.123823518623745,
0.394174530911058));
#8241=CARTESIAN_POINT('Ctrl Pts',(-1.66658649961961,-0.192480977588835,
0.368536561654407));
#8242=CARTESIAN_POINT('Ctrl Pts',(-1.67246562047521,-0.236152929235937,
0.341837165343982));
#8243=CARTESIAN_POINT('Ctrl Pts',(-1.68332504372461,-0.303141259068211,
0.283214707341173));
#8244=CARTESIAN_POINT('Ctrl Pts',(-1.68958170688653,-0.335108247315848,
0.244262842368623));
#8245=CARTESIAN_POINT('Ctrl Pts',(-1.69769003172132,-0.373243761060364,
0.178166559972324));
#8246=CARTESIAN_POINT('Ctrl Pts',(-1.70107730356824,-0.387888272594439,
0.143648558862931));
#8247=CARTESIAN_POINT('Ctrl Pts',(-1.70562212620408,-0.407041111792943,
0.0717778861362656));
#8248=CARTESIAN_POINT('Ctrl Pts',(-1.706752,-0.411552957311693,0.0344244045173313));
#8249=CARTESIAN_POINT('Ctrl Pts',(-1.706752,-0.411552957311693,2.08166817117217E-16));
#8250=CARTESIAN_POINT('',(-1.706752,-0.47628,2.09016837373834E-16));
#8251=CARTESIAN_POINT('',(-1.706752,-0.27783,2.09016837373834E-16));
#8252=CARTESIAN_POINT('Origin',(0.,-0.47628,0.));
#8253=CARTESIAN_POINT('',(-1.65807299932179,-0.07938,-0.404717578595296));
#8254=CARTESIAN_POINT('Ctrl Pts',(-1.706752,-0.411552957311693,2.0122792321331E-16));
#8255=CARTESIAN_POINT('Ctrl Pts',(-1.706752,-0.411552957311693,-0.0344244045173309));
#8256=CARTESIAN_POINT('Ctrl Pts',(-1.70562212620408,-0.407041111792943,
-0.0717778861362652));
#8257=CARTESIAN_POINT('Ctrl Pts',(-1.70107730356824,-0.387888272594439,
-0.143648558862931));
#8258=CARTESIAN_POINT('Ctrl Pts',(-1.69769003172132,-0.373243761060365,
-0.178166559972324));
#8259=CARTESIAN_POINT('Ctrl Pts',(-1.68958170688653,-0.335108247315849,
-0.244262842368623));
#8260=CARTESIAN_POINT('Ctrl Pts',(-1.68332504372461,-0.303141259068212,
-0.283214707341173));
#8261=CARTESIAN_POINT('Ctrl Pts',(-1.67246562047521,-0.236152929235938,
-0.341837165343982));
#8262=CARTESIAN_POINT('Ctrl Pts',(-1.66658649961961,-0.192480977588836,
-0.368536561654407));
#8263=CARTESIAN_POINT('Ctrl Pts',(-1.66063136041479,-0.123823518623745,
-0.394174530911059));
#8264=CARTESIAN_POINT('Ctrl Pts',(-1.65912839404491,-0.101649918886749,
-0.400393769631748));
#8265=CARTESIAN_POINT('Ctrl Pts',(-1.65807299932179,-0.0793800000000001,
-0.404717578595296));
#8266=CARTESIAN_POINT('',(-1.45861320581289,-0.07938,-0.886256117232623));
#8267=CARTESIAN_POINT('Origin',(0.,-0.07938,0.));
#8268=CARTESIAN_POINT('',(-0.886256117232623,-0.07938,-1.45861320581289));
#8269=CARTESIAN_POINT('Ctrl Pts',(-1.45861320581289,-0.0793800000000001,
-0.886256117232623));
#8270=CARTESIAN_POINT('Ctrl Pts',(-1.45630208793976,-0.101649918886749,
-0.890059788636852));
#8271=CARTESIAN_POINT('Ctrl Pts',(-1.45296717977858,-0.123823518623745,
-0.895520212222106));
#8272=CARTESIAN_POINT('Ctrl Pts',(-1.43904931717599,-0.192480977588835,
-0.917859913453974));
#8273=CARTESIAN_POINT('Ctrl Pts',(-1.4243271592157,-0.236152929235937,-0.940896403863072));
#8274=CARTESIAN_POINT('Ctrl Pts',(-1.39055359345152,-0.303141259068212,
-0.990027513266106));
#8275=CARTESIAN_POINT('Ctrl Pts',(-1.36743459453896,-0.335108247315849,
-1.02199477007745));
#8276=CARTESIAN_POINT('Ctrl Pts',(-1.32643091652006,-0.373243761060364,
-1.07446535104584));
#8277=CARTESIAN_POINT('Ctrl Pts',(-1.30441816675528,-0.387888272594439,
-1.10126842659597));
#8278=CARTESIAN_POINT('Ctrl Pts',(-1.25681160160691,-0.407041111792943,
-1.15530234155453));
#8279=CARTESIAN_POINT('Ctrl Pts',(-1.23119764287622,-0.411552957311693,
-1.18251418313119));
#8280=CARTESIAN_POINT('Ctrl Pts',(-1.18251418313119,-0.411552957311693,
-1.23119764287622));
#8281=CARTESIAN_POINT('Ctrl Pts',(-1.15530234155453,-0.407041111792943,
-1.25681160160691));
#8282=CARTESIAN_POINT('Ctrl Pts',(-1.10126842659597,-0.387888272594439,
-1.30441816675528));
#8283=CARTESIAN_POINT('Ctrl Pts',(-1.07446535104584,-0.373243761060364,
-1.32643091652006));
#8284=CARTESIAN_POINT('Ctrl Pts',(-1.02199477007745,-0.335108247315848,
-1.36743459453896));
#8285=CARTESIAN_POINT('Ctrl Pts',(-0.990027513266105,-0.303141259068211,
-1.39055359345152));
#8286=CARTESIAN_POINT('Ctrl Pts',(-0.940896403863071,-0.236152929235936,
-1.42432715921571));
#8287=CARTESIAN_POINT('Ctrl Pts',(-0.917859913453974,-0.192480977588835,
-1.43904931717599));
#8288=CARTESIAN_POINT('Ctrl Pts',(-0.895520212222106,-0.123823518623745,
-1.45296717977858));
#8289=CARTESIAN_POINT('Ctrl Pts',(-0.890059788636851,-0.101649918886749,
-1.45630208793976));
#8290=CARTESIAN_POINT('Ctrl Pts',(-0.886256117232623,-0.0793800000000001,
-1.45861320581289));
#8291=CARTESIAN_POINT('',(-0.404717578595295,-0.07938,-1.65807299932179));
#8292=CARTESIAN_POINT('Origin',(0.,-0.07938,0.));
#8293=CARTESIAN_POINT('',(0.404717578595296,-0.07938,-1.65807299932179));
#8294=CARTESIAN_POINT('Ctrl Pts',(-0.404717578595296,-0.0793800000000001,
-1.65807299932179));
#8295=CARTESIAN_POINT('Ctrl Pts',(-0.400393769631747,-0.101649918886749,
-1.65912839404491));
#8296=CARTESIAN_POINT('Ctrl Pts',(-0.394174530911058,-0.123823518623746,
-1.66063136041479));
#8297=CARTESIAN_POINT('Ctrl Pts',(-0.368536561654407,-0.192480977588836,
-1.66658649961961));
#8298=CARTESIAN_POINT('Ctrl Pts',(-0.341837165343982,-0.236152929235938,
-1.67246562047521));
#8299=CARTESIAN_POINT('Ctrl Pts',(-0.283214707341173,-0.303141259068212,
-1.68332504372461));
#8300=CARTESIAN_POINT('Ctrl Pts',(-0.244262842368623,-0.335108247315849,
-1.68958170688653));
#8301=CARTESIAN_POINT('Ctrl Pts',(-0.178166559972324,-0.373243761060364,
-1.69769003172132));
#8302=CARTESIAN_POINT('Ctrl Pts',(-0.143648558862931,-0.387888272594439,
-1.70107730356824));
#8303=CARTESIAN_POINT('Ctrl Pts',(-0.0717778861362653,-0.407041111792943,
-1.70562212620408));
#8304=CARTESIAN_POINT('Ctrl Pts',(-0.034424404517331,-0.411552957311693,
-1.706752));
#8305=CARTESIAN_POINT('Ctrl Pts',(0.0344244045173312,-0.411552957311693,
-1.706752));
#8306=CARTESIAN_POINT('Ctrl Pts',(0.0717778861362655,-0.407041111792943,
-1.70562212620408));
#8307=CARTESIAN_POINT('Ctrl Pts',(0.143648558862931,-0.387888272594439,
-1.70107730356824));
#8308=CARTESIAN_POINT('Ctrl Pts',(0.178166559972324,-0.373243761060364,
-1.69769003172132));
#8309=CARTESIAN_POINT('Ctrl Pts',(0.244262842368623,-0.335108247315849,
-1.68958170688653));
#8310=CARTESIAN_POINT('Ctrl Pts',(0.283214707341173,-0.303141259068212,
-1.68332504372461));
#8311=CARTESIAN_POINT('Ctrl Pts',(0.341837165343982,-0.236152929235937,
-1.67246562047521));
#8312=CARTESIAN_POINT('Ctrl Pts',(0.368536561654407,-0.192480977588835,
-1.66658649961961));
#8313=CARTESIAN_POINT('Ctrl Pts',(0.394174530911059,-0.123823518623745,
-1.66063136041479));
#8314=CARTESIAN_POINT('Ctrl Pts',(0.400393769631748,-0.101649918886749,
-1.65912839404491));
#8315=CARTESIAN_POINT('Ctrl Pts',(0.404717578595296,-0.0793800000000001,
-1.65807299932179));
#8316=CARTESIAN_POINT('',(0.886256117232623,-0.07938,-1.45861320581289));
#8317=CARTESIAN_POINT('Origin',(0.,-0.07938,0.));
#8318=CARTESIAN_POINT('',(1.45861320581289,-0.07938,-0.886256117232623));
#8319=CARTESIAN_POINT('Ctrl Pts',(0.886256117232623,-0.0793800000000001,
-1.45861320581289));
#8320=CARTESIAN_POINT('Ctrl Pts',(0.890059788636852,-0.101649918886749,
-1.45630208793976));
#8321=CARTESIAN_POINT('Ctrl Pts',(0.895520212222106,-0.123823518623745,
-1.45296717977858));
#8322=CARTESIAN_POINT('Ctrl Pts',(0.917859913453974,-0.192480977588835,
-1.43904931717599));
#8323=CARTESIAN_POINT('Ctrl Pts',(0.940896403863072,-0.236152929235937,
-1.4243271592157));
#8324=CARTESIAN_POINT('Ctrl Pts',(0.990027513266106,-0.303141259068211,
-1.39055359345152));
#8325=CARTESIAN_POINT('Ctrl Pts',(1.02199477007745,-0.335108247315849,-1.36743459453896));
#8326=CARTESIAN_POINT('Ctrl Pts',(1.07446535104584,-0.373243761060364,-1.32643091652006));
#8327=CARTESIAN_POINT('Ctrl Pts',(1.10126842659597,-0.387888272594439,-1.30441816675528));
#8328=CARTESIAN_POINT('Ctrl Pts',(1.15530234155453,-0.407041111792943,-1.25681160160691));
#8329=CARTESIAN_POINT('Ctrl Pts',(1.18251418313119,-0.411552957311693,-1.23119764287622));
#8330=CARTESIAN_POINT('Ctrl Pts',(1.23119764287622,-0.411552957311693,-1.18251418313119));
#8331=CARTESIAN_POINT('Ctrl Pts',(1.25681160160691,-0.407041111792943,-1.15530234155453));
#8332=CARTESIAN_POINT('Ctrl Pts',(1.30441816675528,-0.387888272594439,-1.10126842659597));
#8333=CARTESIAN_POINT('Ctrl Pts',(1.32643091652006,-0.373243761060364,-1.07446535104584));
#8334=CARTESIAN_POINT('Ctrl Pts',(1.36743459453896,-0.335108247315849,-1.02199477007745));
#8335=CARTESIAN_POINT('Ctrl Pts',(1.39055359345152,-0.303141259068212,-0.990027513266105));
#8336=CARTESIAN_POINT('Ctrl Pts',(1.4243271592157,-0.236152929235937,-0.940896403863071));
#8337=CARTESIAN_POINT('Ctrl Pts',(1.43904931717599,-0.192480977588835,-0.917859913453974));
#8338=CARTESIAN_POINT('Ctrl Pts',(1.45296717977858,-0.123823518623745,-0.895520212222106));
#8339=CARTESIAN_POINT('Ctrl Pts',(1.45630208793976,-0.101649918886749,-0.890059788636852));
#8340=CARTESIAN_POINT('Ctrl Pts',(1.45861320581289,-0.0793800000000001,
-0.886256117232623));
#8341=CARTESIAN_POINT('',(1.65807299932179,-0.07938,-0.404717578595296));
#8342=CARTESIAN_POINT('Origin',(0.,-0.07938,0.));
#8343=CARTESIAN_POINT('',(1.65807299932179,-0.07938,0.404717578595296));
#8344=CARTESIAN_POINT('Ctrl Pts',(1.65807299932179,-0.0793800000000001,
-0.404717578595296));
#8345=CARTESIAN_POINT('Ctrl Pts',(1.65912839404491,-0.101649918886749,-0.400393769631747));
#8346=CARTESIAN_POINT('Ctrl Pts',(1.66063136041479,-0.123823518623745,-0.394174530911058));
#8347=CARTESIAN_POINT('Ctrl Pts',(1.66658649961961,-0.192480977588835,-0.368536561654407));
#8348=CARTESIAN_POINT('Ctrl Pts',(1.67246562047521,-0.236152929235937,-0.341837165343982));
#8349=CARTESIAN_POINT('Ctrl Pts',(1.68332504372461,-0.303141259068212,-0.283214707341173));
#8350=CARTESIAN_POINT('Ctrl Pts',(1.68958170688653,-0.335108247315849,-0.244262842368623));
#8351=CARTESIAN_POINT('Ctrl Pts',(1.69769003172132,-0.373243761060364,-0.178166559972324));
#8352=CARTESIAN_POINT('Ctrl Pts',(1.70107730356824,-0.387888272594439,-0.143648558862931));
#8353=CARTESIAN_POINT('Ctrl Pts',(1.70562212620408,-0.407041111792943,-0.0717778861362655));
#8354=CARTESIAN_POINT('Ctrl Pts',(1.706752,-0.411552957311693,-0.0344244045173312));
#8355=CARTESIAN_POINT('Ctrl Pts',(1.706752,-0.411552957311693,0.0344244045173312));
#8356=CARTESIAN_POINT('Ctrl Pts',(1.70562212620408,-0.407041111792943,0.0717778861362655));
#8357=CARTESIAN_POINT('Ctrl Pts',(1.70107730356824,-0.387888272594439,0.143648558862931));
#8358=CARTESIAN_POINT('Ctrl Pts',(1.69769003172132,-0.373243761060364,0.178166559972324));
#8359=CARTESIAN_POINT('Ctrl Pts',(1.68958170688653,-0.335108247315849,0.244262842368623));
#8360=CARTESIAN_POINT('Ctrl Pts',(1.68332504372461,-0.303141259068212,0.283214707341173));
#8361=CARTESIAN_POINT('Ctrl Pts',(1.67246562047521,-0.236152929235937,0.341837165343982));
#8362=CARTESIAN_POINT('Ctrl Pts',(1.66658649961961,-0.192480977588835,0.368536561654407));
#8363=CARTESIAN_POINT('Ctrl Pts',(1.66063136041479,-0.123823518623745,0.394174530911058));
#8364=CARTESIAN_POINT('Ctrl Pts',(1.65912839404491,-0.101649918886749,0.400393769631747));
#8365=CARTESIAN_POINT('Ctrl Pts',(1.65807299932179,-0.0793800000000001,
0.404717578595296));
#8366=CARTESIAN_POINT('Origin',(0.,-0.07938,0.));
#8367=CARTESIAN_POINT('Origin',(0.,-0.07938,0.));
#8368=CARTESIAN_POINT('',(0.397005914195118,-0.07938,1.59456899932179));
#8369=CARTESIAN_POINT('Origin',(0.,-0.07938,0.));
#8370=CARTESIAN_POINT('Origin',(-3.33066907387547E-16,-0.07938,1.675));
#8371=CARTESIAN_POINT('Origin',(-3.33066907387547E-16,0.,1.675));
#8372=CARTESIAN_POINT('',(-0.397005914195118,-0.07938,1.59456899932179));
#8373=CARTESIAN_POINT('Ctrl Pts',(-0.397005914195119,-0.0793800000000001,
1.59456899932179));
#8374=CARTESIAN_POINT('Ctrl Pts',(-0.3886265584581,-0.123401821157026,1.59665523941937));
#8375=CARTESIAN_POINT('Ctrl Pts',(-0.373030350867485,-0.166543350814306,
1.60050712143809));
#8376=CARTESIAN_POINT('Ctrl Pts',(-0.333298652394954,-0.237231147975234,
1.60919314384089));
#8377=CARTESIAN_POINT('Ctrl Pts',(-0.311480544243687,-0.266264900654909,
1.61365775139403));
#8378=CARTESIAN_POINT('Ctrl Pts',(-0.261368388670537,-0.317195968905306,
1.62252828437015));
#8379=CARTESIAN_POINT('Ctrl Pts',(-0.233069203882014,-0.33909093068465,
1.62691869420078));
#8380=CARTESIAN_POINT('Ctrl Pts',(-0.174042761838764,-0.373586846396559,
1.63426473152765));
#8381=CARTESIAN_POINT('Ctrl Pts',(-0.14036578147155,-0.388086240756494,
1.63761964365402));
#8382=CARTESIAN_POINT('Ctrl Pts',(-0.0701778381840615,-0.407068917407805,
1.64212536811722));
#8383=CARTESIAN_POINT('Ctrl Pts',(-0.0336652739555918,-0.411552957311693,
1.643248));
#8384=CARTESIAN_POINT('Ctrl Pts',(0.0336652739555913,-0.411552957311693,
1.643248));
#8385=CARTESIAN_POINT('Ctrl Pts',(0.070177838184061,-0.407068917407805,
1.64212536811722));
#8386=CARTESIAN_POINT('Ctrl Pts',(0.140365781471549,-0.388086240756494,
1.63761964365402));
#8387=CARTESIAN_POINT('Ctrl Pts',(0.174042761838763,-0.373586846396559,
1.63426473152765));
#8388=CARTESIAN_POINT('Ctrl Pts',(0.233069203882014,-0.33909093068465,1.62691869420078));
#8389=CARTESIAN_POINT('Ctrl Pts',(0.261368388670536,-0.317195968905306,
1.62252828437015));
#8390=CARTESIAN_POINT('Ctrl Pts',(0.311480544243686,-0.266264900654908,
1.61365775139403));
#8391=CARTESIAN_POINT('Ctrl Pts',(0.333298652394954,-0.237231147975234,
1.60919314384089));
#8392=CARTESIAN_POINT('Ctrl Pts',(0.373030350867484,-0.166543350814306,
1.60050712143809));
#8393=CARTESIAN_POINT('Ctrl Pts',(0.388626558458099,-0.123401821157026,
1.59665523941937));
#8394=CARTESIAN_POINT('Ctrl Pts',(0.397005914195118,-0.07938,1.59456899932179));
#8395=CARTESIAN_POINT('Origin',(-3.33066907387547E-16,-0.07938,1.675));
#8396=CARTESIAN_POINT('Origin',(0.,-0.07938,0.));
#8397=CARTESIAN_POINT('',(-0.846804978391754,-0.07938,1.40825612658882));
#8398=CARTESIAN_POINT('Origin',(0.,-0.07938,0.));
#8399=CARTESIAN_POINT('Origin',(-1.18440385848747,-0.07938,1.18440385848747));
#8400=CARTESIAN_POINT('Origin',(-1.18440385848747,0.,1.18440385848747));
#8401=CARTESIAN_POINT('',(-1.40825612658882,-0.07938,0.846804978391753));
#8402=CARTESIAN_POINT('Ctrl Pts',(-1.40825612658882,-0.0793800000000001,
0.846804978391753));
#8403=CARTESIAN_POINT('Ctrl Pts',(-1.40380622184538,-0.123401821157026,
0.854205272175555));
#8404=CARTESIAN_POINT('Ctrl Pts',(-1.39550172959303,-0.166543350814306,
0.867957148219442));
#8405=CARTESIAN_POINT('Ctrl Pts',(-1.3735491215176,-0.237231147975235,0.902193646979983));
#8406=CARTESIAN_POINT('Ctrl Pts',(-1.36127834356734,-0.266264900654909,
0.920778333482565));
#8407=CARTESIAN_POINT('Ctrl Pts',(-1.33211611256184,-0.317195968905306,
0.962485392528369));
#8408=CARTESIAN_POINT('Ctrl Pts',(-1.31521005565926,-0.339090930684651,
0.985600426557816));
#8409=CARTESIAN_POINT('Ctrl Pts',(-1.27866649102984,-0.373586846396559,
1.03253285680459));
#8410=CARTESIAN_POINT('Ctrl Pts',(-1.25722555095714,-0.388086240756494,
1.05871835910697));
#8411=CARTESIAN_POINT('Ctrl Pts',(-1.2107812086231,-0.407068917407805,1.11153475808518));
#8412=CARTESIAN_POINT('Ctrl Pts',(-1.18575674747573,-0.411552957311693,
1.13814686046673));
#8413=CARTESIAN_POINT('Ctrl Pts',(-1.13814686046673,-0.411552957311693,
1.18575674747573));
#8414=CARTESIAN_POINT('Ctrl Pts',(-1.11153475808518,-0.407068917407805,
1.2107812086231));
#8415=CARTESIAN_POINT('Ctrl Pts',(-1.05871835910697,-0.388086240756494,
1.25722555095714));
#8416=CARTESIAN_POINT('Ctrl Pts',(-1.03253285680459,-0.373586846396559,
1.27866649102984));
#8417=CARTESIAN_POINT('Ctrl Pts',(-0.985600426557816,-0.33909093068465,
1.31521005565926));
#8418=CARTESIAN_POINT('Ctrl Pts',(-0.962485392528369,-0.317195968905306,
1.33211611256184));
#8419=CARTESIAN_POINT('Ctrl Pts',(-0.920778333482565,-0.266264900654908,
1.36127834356734));
#8420=CARTESIAN_POINT('Ctrl Pts',(-0.902193646979983,-0.237231147975234,
1.3735491215176));
#8421=CARTESIAN_POINT('Ctrl Pts',(-0.867957148219442,-0.166543350814306,
1.39550172959303));
#8422=CARTESIAN_POINT('Ctrl Pts',(-0.854205272175555,-0.123401821157026,
1.40380622184538));
#8423=CARTESIAN_POINT('Ctrl Pts',(-0.846804978391753,-0.0793800000000001,
1.40825612658882));
#8424=CARTESIAN_POINT('Origin',(-1.18440385848747,-0.07938,1.18440385848747));
#8425=CARTESIAN_POINT('Origin',(0.,-0.07938,0.));
#8426=CARTESIAN_POINT('',(-1.59456899932179,-0.07938,0.397005914195118));
#8427=CARTESIAN_POINT('Origin',(0.,-0.07938,0.));
#8428=CARTESIAN_POINT('Origin',(-1.675,-0.07938,-2.22044604925031E-16));
#8429=CARTESIAN_POINT('Origin',(-1.675,0.,-2.22044604925031E-16));
#8430=CARTESIAN_POINT('',(-1.59456899932179,-0.07938,-0.397005914195118));
#8431=CARTESIAN_POINT('',(-1.643248,-0.411552957311693,3.47540551556327E-18));
#8432=CARTESIAN_POINT('Ctrl Pts',(-1.59456899932179,-0.0793800000000001,
-0.397005914195119));
#8433=CARTESIAN_POINT('Ctrl Pts',(-1.59665523941937,-0.123401821157026,
-0.388626558458099));
#8434=CARTESIAN_POINT('Ctrl Pts',(-1.60050712143809,-0.166543350814306,
-0.373030350867485));
#8435=CARTESIAN_POINT('Ctrl Pts',(-1.60919314384089,-0.237231147975234,
-0.333298652394954));
#8436=CARTESIAN_POINT('Ctrl Pts',(-1.61365775139403,-0.266264900654909,
-0.311480544243686));
#8437=CARTESIAN_POINT('Ctrl Pts',(-1.62252828437015,-0.317195968905306,
-0.261368388670537));
#8438=CARTESIAN_POINT('Ctrl Pts',(-1.62691869420078,-0.33909093068465,-0.233069203882014));
#8439=CARTESIAN_POINT('Ctrl Pts',(-1.63426473152765,-0.373586846396559,
-0.174042761838764));
#8440=CARTESIAN_POINT('Ctrl Pts',(-1.63761964365402,-0.388086240756494,
-0.140365781471549));
#8441=CARTESIAN_POINT('Ctrl Pts',(-1.64212536811722,-0.407068917407805,
-0.0701778381840614));
#8442=CARTESIAN_POINT('Ctrl Pts',(-1.643248,-0.411552957311693,-0.0336652739555917));
#8443=CARTESIAN_POINT('Ctrl Pts',(-1.643248,-0.411552957311693,-2.0122792321331E-16));
#8444=CARTESIAN_POINT('Origin',(-1.675,-0.07938,-2.22044604925031E-16));
#8445=CARTESIAN_POINT('Ctrl Pts',(-1.643248,-0.411552957311693,-1.94289029309402E-16));
#8446=CARTESIAN_POINT('Ctrl Pts',(-1.643248,-0.411552957311693,0.0336652739555913));
#8447=CARTESIAN_POINT('Ctrl Pts',(-1.64212536811722,-0.407068917407805,
0.0701778381840609));
#8448=CARTESIAN_POINT('Ctrl Pts',(-1.63761964365402,-0.388086240756494,
0.140365781471549));
#8449=CARTESIAN_POINT('Ctrl Pts',(-1.63426473152765,-0.373586846396559,
0.174042761838763));
#8450=CARTESIAN_POINT('Ctrl Pts',(-1.62691869420078,-0.33909093068465,0.233069203882014));
#8451=CARTESIAN_POINT('Ctrl Pts',(-1.62252828437015,-0.317195968905306,
0.261368388670536));
#8452=CARTESIAN_POINT('Ctrl Pts',(-1.61365775139403,-0.266264900654909,
0.311480544243686));
#8453=CARTESIAN_POINT('Ctrl Pts',(-1.60919314384089,-0.237231147975235,
0.333298652394954));
#8454=CARTESIAN_POINT('Ctrl Pts',(-1.60050712143809,-0.166543350814306,
0.373030350867484));
#8455=CARTESIAN_POINT('Ctrl Pts',(-1.59665523941937,-0.123401821157026,
0.388626558458099));
#8456=CARTESIAN_POINT('Ctrl Pts',(-1.59456899932179,-0.0793800000000001,
0.397005914195118));
#8457=CARTESIAN_POINT('Origin',(0.,-0.07938,0.));
#8458=CARTESIAN_POINT('',(-1.40825612658882,-0.07938,-0.846804978391753));
#8459=CARTESIAN_POINT('Origin',(0.,-0.07938,0.));
#8460=CARTESIAN_POINT('Origin',(-1.18440385848747,-0.07938,-1.18440385848747));
#8461=CARTESIAN_POINT('Origin',(-1.18440385848747,0.,-1.18440385848747));
#8462=CARTESIAN_POINT('',(-0.846804978391753,-0.07938,-1.40825612658882));
#8463=CARTESIAN_POINT('Ctrl Pts',(-0.846804978391753,-0.0793800000000001,
-1.40825612658882));
#8464=CARTESIAN_POINT('Ctrl Pts',(-0.854205272175555,-0.123401821157026,
-1.40380622184538));
#8465=CARTESIAN_POINT('Ctrl Pts',(-0.867957148219442,-0.166543350814306,
-1.39550172959303));
#8466=CARTESIAN_POINT('Ctrl Pts',(-0.902193646979982,-0.237231147975234,
-1.3735491215176));
#8467=CARTESIAN_POINT('Ctrl Pts',(-0.920778333482564,-0.266264900654908,
-1.36127834356734));
#8468=CARTESIAN_POINT('Ctrl Pts',(-0.962485392528368,-0.317195968905306,
-1.33211611256184));
#8469=CARTESIAN_POINT('Ctrl Pts',(-0.985600426557816,-0.33909093068465,
-1.31521005565926));
#8470=CARTESIAN_POINT('Ctrl Pts',(-1.03253285680459,-0.373586846396559,
-1.27866649102984));
#8471=CARTESIAN_POINT('Ctrl Pts',(-1.05871835910697,-0.388086240756494,
-1.25722555095714));
#8472=CARTESIAN_POINT('Ctrl Pts',(-1.11153475808518,-0.407068917407805,
-1.2107812086231));
#8473=CARTESIAN_POINT('Ctrl Pts',(-1.13814686046673,-0.411552957311693,
-1.18575674747573));
#8474=CARTESIAN_POINT('Ctrl Pts',(-1.18575674747573,-0.411552957311693,
-1.13814686046673));
#8475=CARTESIAN_POINT('Ctrl Pts',(-1.2107812086231,-0.407068917407805,-1.11153475808518));
#8476=CARTESIAN_POINT('Ctrl Pts',(-1.25722555095714,-0.388086240756494,
-1.05871835910697));
#8477=CARTESIAN_POINT('Ctrl Pts',(-1.27866649102984,-0.373586846396559,
-1.03253285680459));
#8478=CARTESIAN_POINT('Ctrl Pts',(-1.31521005565926,-0.33909093068465,-0.985600426557816));
#8479=CARTESIAN_POINT('Ctrl Pts',(-1.33211611256184,-0.317195968905306,
-0.962485392528369));
#8480=CARTESIAN_POINT('Ctrl Pts',(-1.36127834356734,-0.266264900654909,
-0.920778333482565));
#8481=CARTESIAN_POINT('Ctrl Pts',(-1.3735491215176,-0.237231147975234,-0.902193646979983));
#8482=CARTESIAN_POINT('Ctrl Pts',(-1.39550172959303,-0.166543350814306,
-0.867957148219442));
#8483=CARTESIAN_POINT('Ctrl Pts',(-1.40380622184538,-0.123401821157026,
-0.854205272175555));
#8484=CARTESIAN_POINT('Ctrl Pts',(-1.40825612658882,-0.07938,-0.846804978391753));
#8485=CARTESIAN_POINT('Origin',(-1.18440385848747,-0.07938,-1.18440385848747));
#8486=CARTESIAN_POINT('Origin',(0.,-0.07938,0.));
#8487=CARTESIAN_POINT('',(-0.397005914195118,-0.07938,-1.59456899932179));
#8488=CARTESIAN_POINT('Origin',(0.,-0.07938,0.));
#8489=CARTESIAN_POINT('Origin',(1.11022302462516E-16,-0.07938,-1.675));
#8490=CARTESIAN_POINT('Origin',(1.11022302462516E-16,0.,-1.675));
#8491=CARTESIAN_POINT('',(0.397005914195118,-0.07938,-1.59456899932179));
#8492=CARTESIAN_POINT('Ctrl Pts',(0.397005914195119,-0.0793800000000001,
-1.59456899932179));
#8493=CARTESIAN_POINT('Ctrl Pts',(0.388626558458099,-0.123401821157026,
-1.59665523941937));
#8494=CARTESIAN_POINT('Ctrl Pts',(0.373030350867485,-0.166543350814306,
-1.60050712143809));
#8495=CARTESIAN_POINT('Ctrl Pts',(0.333298652394954,-0.237231147975234,
-1.60919314384089));
#8496=CARTESIAN_POINT('Ctrl Pts',(0.311480544243686,-0.266264900654909,
-1.61365775139403));
#8497=CARTESIAN_POINT('Ctrl Pts',(0.261368388670537,-0.317195968905306,
-1.62252828437015));
#8498=CARTESIAN_POINT('Ctrl Pts',(0.233069203882014,-0.33909093068465,-1.62691869420078));
#8499=CARTESIAN_POINT('Ctrl Pts',(0.174042761838763,-0.373586846396559,
-1.63426473152765));
#8500=CARTESIAN_POINT('Ctrl Pts',(0.140365781471549,-0.388086240756494,
-1.63761964365402));
#8501=CARTESIAN_POINT('Ctrl Pts',(0.0701778381840612,-0.407068917407805,
-1.64212536811722));
#8502=CARTESIAN_POINT('Ctrl Pts',(0.0336652739555916,-0.411552957311693,
-1.643248));
#8503=CARTESIAN_POINT('Ctrl Pts',(-0.0336652739555915,-0.411552957311693,
-1.643248));
#8504=CARTESIAN_POINT('Ctrl Pts',(-0.0701778381840612,-0.407068917407805,
-1.64212536811722));
#8505=CARTESIAN_POINT('Ctrl Pts',(-0.140365781471549,-0.388086240756494,
-1.63761964365402));
#8506=CARTESIAN_POINT('Ctrl Pts',(-0.174042761838764,-0.373586846396559,
-1.63426473152765));
#8507=CARTESIAN_POINT('Ctrl Pts',(-0.233069203882014,-0.33909093068465,
-1.62691869420078));
#8508=CARTESIAN_POINT('Ctrl Pts',(-0.261368388670536,-0.317195968905306,
-1.62252828437015));
#8509=CARTESIAN_POINT('Ctrl Pts',(-0.311480544243686,-0.266264900654908,
-1.61365775139403));
#8510=CARTESIAN_POINT('Ctrl Pts',(-0.333298652394954,-0.237231147975234,
-1.60919314384089));
#8511=CARTESIAN_POINT('Ctrl Pts',(-0.373030350867485,-0.166543350814306,
-1.60050712143809));
#8512=CARTESIAN_POINT('Ctrl Pts',(-0.388626558458099,-0.123401821157026,
-1.59665523941937));
#8513=CARTESIAN_POINT('Ctrl Pts',(-0.397005914195118,-0.07938,-1.59456899932179));
#8514=CARTESIAN_POINT('Origin',(1.11022302462516E-16,-0.07938,-1.675));
#8515=CARTESIAN_POINT('Origin',(0.,-0.07938,0.));
#8516=CARTESIAN_POINT('',(0.846804978391753,-0.07938,-1.40825612658882));
#8517=CARTESIAN_POINT('Origin',(0.,-0.07938,0.));
#8518=CARTESIAN_POINT('Origin',(1.18440385848747,-0.07938,-1.18440385848747));
#8519=CARTESIAN_POINT('Origin',(1.18440385848747,0.,-1.18440385848747));
#8520=CARTESIAN_POINT('',(1.40825612658882,-0.07938,-0.846804978391753));
#8521=CARTESIAN_POINT('Ctrl Pts',(1.40825612658882,-0.0793800000000001,
-0.846804978391753));
#8522=CARTESIAN_POINT('Ctrl Pts',(1.40380622184538,-0.123401821157026,-0.854205272175555));
#8523=CARTESIAN_POINT('Ctrl Pts',(1.39550172959303,-0.166543350814306,-0.867957148219442));
#8524=CARTESIAN_POINT('Ctrl Pts',(1.3735491215176,-0.237231147975234,-0.902193646979983));
#8525=CARTESIAN_POINT('Ctrl Pts',(1.36127834356734,-0.266264900654908,-0.920778333482565));
#8526=CARTESIAN_POINT('Ctrl Pts',(1.33211611256184,-0.317195968905306,-0.962485392528369));
#8527=CARTESIAN_POINT('Ctrl Pts',(1.31521005565926,-0.33909093068465,-0.985600426557816));
#8528=CARTESIAN_POINT('Ctrl Pts',(1.27866649102984,-0.373586846396559,-1.03253285680459));
#8529=CARTESIAN_POINT('Ctrl Pts',(1.25722555095714,-0.388086240756494,-1.05871835910697));
#8530=CARTESIAN_POINT('Ctrl Pts',(1.2107812086231,-0.407068917407805,-1.11153475808518));
#8531=CARTESIAN_POINT('Ctrl Pts',(1.18575674747573,-0.411552957311693,-1.13814686046673));
#8532=CARTESIAN_POINT('Ctrl Pts',(1.13814686046673,-0.411552957311693,-1.18575674747573));
#8533=CARTESIAN_POINT('Ctrl Pts',(1.11153475808518,-0.407068917407805,-1.2107812086231));
#8534=CARTESIAN_POINT('Ctrl Pts',(1.05871835910697,-0.388086240756494,-1.25722555095714));
#8535=CARTESIAN_POINT('Ctrl Pts',(1.03253285680459,-0.373586846396559,-1.27866649102984));
#8536=CARTESIAN_POINT('Ctrl Pts',(0.985600426557816,-0.33909093068465,-1.31521005565926));
#8537=CARTESIAN_POINT('Ctrl Pts',(0.962485392528369,-0.317195968905306,
-1.33211611256184));
#8538=CARTESIAN_POINT('Ctrl Pts',(0.920778333482565,-0.266264900654909,
-1.36127834356734));
#8539=CARTESIAN_POINT('Ctrl Pts',(0.902193646979983,-0.237231147975234,
-1.3735491215176));
#8540=CARTESIAN_POINT('Ctrl Pts',(0.867957148219442,-0.166543350814306,
-1.39550172959303));
#8541=CARTESIAN_POINT('Ctrl Pts',(0.854205272175555,-0.123401821157026,
-1.40380622184538));
#8542=CARTESIAN_POINT('Ctrl Pts',(0.846804978391753,-0.0793800000000001,
-1.40825612658882));
#8543=CARTESIAN_POINT('Origin',(1.18440385848747,-0.07938,-1.18440385848747));
#8544=CARTESIAN_POINT('Origin',(0.,-0.27783,0.));
#8545=CARTESIAN_POINT('',(-1.643248,-0.47628,2.01239840340529E-16));
#8546=CARTESIAN_POINT('Origin',(0.,-0.47628,0.));
#8547=CARTESIAN_POINT('',(-1.643248,-0.27783,2.01239840340529E-16));
#8548=CARTESIAN_POINT('',(1.59456899932179,-0.07938,0.397005914195118));
#8549=CARTESIAN_POINT('Origin',(0.,-0.07938,0.));
#8550=CARTESIAN_POINT('',(1.59456899932179,-0.07938,-0.397005914195118));
#8551=CARTESIAN_POINT('Ctrl Pts',(1.59456899932179,-0.0793800000000001,
0.397005914195118));
#8552=CARTESIAN_POINT('Ctrl Pts',(1.59665523941937,-0.123401821157026,0.388626558458099));
#8553=CARTESIAN_POINT('Ctrl Pts',(1.60050712143809,-0.166543350814306,0.373030350867485));
#8554=CARTESIAN_POINT('Ctrl Pts',(1.60919314384089,-0.237231147975234,0.333298652394954));
#8555=CARTESIAN_POINT('Ctrl Pts',(1.61365775139403,-0.266264900654909,0.311480544243686));
#8556=CARTESIAN_POINT('Ctrl Pts',(1.62252828437015,-0.317195968905306,0.261368388670537));
#8557=CARTESIAN_POINT('Ctrl Pts',(1.62691869420078,-0.33909093068465,0.233069203882014));
#8558=CARTESIAN_POINT('Ctrl Pts',(1.63426473152765,-0.373586846396559,0.174042761838764));
#8559=CARTESIAN_POINT('Ctrl Pts',(1.63761964365402,-0.388086240756494,0.140365781471549));
#8560=CARTESIAN_POINT('Ctrl Pts',(1.64212536811722,-0.407068917407805,0.0701778381840612));
#8561=CARTESIAN_POINT('Ctrl Pts',(1.643248,-0.411552957311693,0.0336652739555916));
#8562=CARTESIAN_POINT('Ctrl Pts',(1.643248,-0.411552957311693,-0.0336652739555916));
#8563=CARTESIAN_POINT('Ctrl Pts',(1.64212536811722,-0.407068917407805,-0.0701778381840612));
#8564=CARTESIAN_POINT('Ctrl Pts',(1.63761964365402,-0.388086240756494,-0.140365781471549));
#8565=CARTESIAN_POINT('Ctrl Pts',(1.63426473152765,-0.373586846396559,-0.174042761838764));
#8566=CARTESIAN_POINT('Ctrl Pts',(1.62691869420078,-0.33909093068465,-0.233069203882014));
#8567=CARTESIAN_POINT('Ctrl Pts',(1.62252828437015,-0.317195968905306,-0.261368388670537));
#8568=CARTESIAN_POINT('Ctrl Pts',(1.61365775139403,-0.266264900654909,-0.311480544243686));
#8569=CARTESIAN_POINT('Ctrl Pts',(1.60919314384089,-0.237231147975234,-0.333298652394954));
#8570=CARTESIAN_POINT('Ctrl Pts',(1.60050712143809,-0.166543350814306,-0.373030350867485));
#8571=CARTESIAN_POINT('Ctrl Pts',(1.59665523941937,-0.123401821157026,-0.388626558458099));
#8572=CARTESIAN_POINT('Ctrl Pts',(1.59456899932179,-0.07938,-0.397005914195118));
#8573=CARTESIAN_POINT('Origin',(0.,-0.07938,0.));
#8574=CARTESIAN_POINT('Origin',(0.,-0.07938,0.));
#8575=CARTESIAN_POINT('Origin',(1.675,-0.07938,0.));
#8576=CARTESIAN_POINT('Origin',(1.675,0.,0.));
#8577=CARTESIAN_POINT('Origin',(1.675,-0.07938,0.));
#8578=CARTESIAN_POINT('Origin',(0.,-0.47628,0.));
#8579=CARTESIAN_POINT('Origin',(0.,-0.07938,0.));
#8580=CARTESIAN_POINT('',(0.,0.,0.));
#8581=CARTESIAN_POINT('Origin',(1.70469,0.695,0.));
#8582=CARTESIAN_POINT('',(-1.70469,0.695,-2.0876431520385E-16));
#8583=CARTESIAN_POINT('Origin',(0.,0.695,0.));
#8584=CARTESIAN_POINT('',(-1.65031,0.695,-2.02104685910087E-16));
#8585=CARTESIAN_POINT('Origin',(0.,0.695,0.));
#8586=CARTESIAN_POINT('Origin',(0.,0.6575,0.));
#8587=CARTESIAN_POINT('',(-1.70469,0.62,-2.0876431520385E-16));
#8588=CARTESIAN_POINT('Origin',(0.,0.62,0.));
#8589=CARTESIAN_POINT('',(-1.70469,0.6575,-2.0876431520385E-16));
#8590=CARTESIAN_POINT('Origin',(1.65031,0.62,0.));
#8591=CARTESIAN_POINT('',(-1.65031,0.62,-2.02104685910087E-16));
#8592=CARTESIAN_POINT('Origin',(0.,0.62,0.));
#8593=CARTESIAN_POINT('Origin',(0.,0.6575,0.));
#8594=CARTESIAN_POINT('',(-1.65031,0.6575,-2.02104685910087E-16));
#8595=CARTESIAN_POINT('Origin',(1.70469,-0.62,0.));
#8596=CARTESIAN_POINT('',(-1.70469,-0.62,-2.0876431520385E-16));
#8597=CARTESIAN_POINT('Origin',(0.,-0.62,0.));
#8598=CARTESIAN_POINT('',(-1.65031,-0.62,-2.02104685910087E-16));
#8599=CARTESIAN_POINT('Origin',(0.,-0.62,0.));
#8600=CARTESIAN_POINT('Origin',(0.,-0.6575,0.));
#8601=CARTESIAN_POINT('',(-1.70469,-0.695,-2.0876431520385E-16));
#8602=CARTESIAN_POINT('Origin',(0.,-0.695,0.));
#8603=CARTESIAN_POINT('',(-1.70469,-0.6575,-2.0876431520385E-16));
#8604=CARTESIAN_POINT('Origin',(1.65031,-0.695,0.));
#8605=CARTESIAN_POINT('',(-1.65031,-0.695,-2.02104685910087E-16));
#8606=CARTESIAN_POINT('Origin',(0.,-0.695,0.));
#8607=CARTESIAN_POINT('Origin',(0.,-0.6575,0.));
#8608=CARTESIAN_POINT('',(-1.65031,-0.6575,-2.02104685910087E-16));
#8609=CARTESIAN_POINT('',(0.,0.,0.));
#8610=CARTESIAN_POINT('',(0.,0.,0.));
#8611=CARTESIAN_POINT('',(0.,0.,0.));
#8612=CARTESIAN_POINT('',(0.,0.,0.));
#8613=CARTESIAN_POINT('',(0.,0.,0.));
#8614=CARTESIAN_POINT('',(0.,0.,0.));
#8615=CARTESIAN_POINT('Origin',(0.45,0.6,0.));
#8616=CARTESIAN_POINT('',(-0.45,0.6,-5.51091059616309E-17));
#8617=CARTESIAN_POINT('Origin',(0.,0.6,0.));
#8618=CARTESIAN_POINT('Origin',(0.,0.575,0.));
#8619=CARTESIAN_POINT('',(-0.5,0.55,-6.12323399573677E-17));
#8620=CARTESIAN_POINT('Origin',(0.,0.55,0.));
#8621=CARTESIAN_POINT('',(-0.475,0.575,-5.81707229594993E-17));
#8622=CARTESIAN_POINT('Origin',(0.,0.29,0.));
#8623=CARTESIAN_POINT('',(-0.5,0.0299999999999998,-6.12323399573677E-17));
#8624=CARTESIAN_POINT('Origin',(0.,0.0299999999999998,0.));
#8625=CARTESIAN_POINT('',(-0.5,0.29,-6.12323399573677E-17));
#8626=CARTESIAN_POINT('Origin',(0.,0.0150000000000001,0.));
#8627=CARTESIAN_POINT('',(-0.47,7.11236625150491E-17,-5.75583995599256E-17));
#8628=CARTESIAN_POINT('Origin',(0.,0.,0.));
#8629=CARTESIAN_POINT('',(-0.485,0.0150000000000001,-5.93953697586466E-17));
#8630=CARTESIAN_POINT('Origin',(0.32,0.,0.));
#8631=CARTESIAN_POINT('',(-0.32,-6.93889390390723E-18,-3.91886975727153E-17));
#8632=CARTESIAN_POINT('Origin',(0.,0.,0.));
#8633=CARTESIAN_POINT('Origin',(0.,-0.02,0.));
#8634=CARTESIAN_POINT('',(-0.2942,-0.0515999999999999,3.60291088309151E-17));
#8635=CARTESIAN_POINT('Origin',(0.,-0.0515999999999999,0.));
#8636=CARTESIAN_POINT('',(-0.31,-0.02,-3.7964050773568E-17));
#8637=CARTESIAN_POINT('Origin',(0.,-1.24,0.));
#8638=CARTESIAN_POINT('',(-0.2942,-2.4458,3.60291088309151E-17));
#8639=CARTESIAN_POINT('Origin',(0.,-2.4458,0.));
#8640=CARTESIAN_POINT('',(-0.2942,-1.24,-3.60291088309151E-17));
#8641=CARTESIAN_POINT('Origin',(0.,-2.47,0.));
#8642=CARTESIAN_POINT('',(-0.24,-2.5,-2.93915231795365E-17));
#8643=CARTESIAN_POINT('Origin',(0.,-2.5,0.));
#8644=CARTESIAN_POINT('',(-0.27,-2.47,-3.30654635769785E-17));
#8645=CARTESIAN_POINT('Origin',(0.,-2.5,0.));
#8646=CARTESIAN_POINT('Origin',(0.144337567297406,-0.6,-0.25));
#8647=CARTESIAN_POINT('',(0.288675134594813,-0.6,0.));
#8648=CARTESIAN_POINT('',(0.144337567297406,-0.6,-0.25));
#8649=CARTESIAN_POINT('',(0.288675134594813,-0.6,0.));
#8650=CARTESIAN_POINT('',(0.144337567297406,-0.96,-0.25));
#8651=CARTESIAN_POINT('',(0.144337567297406,-0.6,-0.25));
#8652=CARTESIAN_POINT('',(0.288675134594813,-0.96,0.));
#8653=CARTESIAN_POINT('',(0.288675134594813,-0.96,0.));
#8654=CARTESIAN_POINT('',(0.288675134594813,-0.6,0.));
#8655=CARTESIAN_POINT('Origin',(-0.144337567297406,-0.6,-0.25));
#8656=CARTESIAN_POINT('',(-0.144337567297406,-0.6,-0.25));
#8657=CARTESIAN_POINT('',(0.144337567297406,-0.6,-0.25));
#8658=CARTESIAN_POINT('',(-0.144337567297406,-0.96,-0.25));
#8659=CARTESIAN_POINT('',(-0.144337567297406,-0.6,-0.25));
#8660=CARTESIAN_POINT('',(0.144337567297406,-0.96,-0.25));
#8661=CARTESIAN_POINT('Origin',(-0.288675134594813,-0.6,-8.32667268468867E-17));
#8662=CARTESIAN_POINT('',(-0.288675134594813,-0.6,-3.53525079574969E-17));
#8663=CARTESIAN_POINT('',(-0.144337567297406,-0.6,-0.25));
#8664=CARTESIAN_POINT('',(-0.288675134594813,-0.96,-5.55111512312578E-17));
#8665=CARTESIAN_POINT('',(-0.288675134594813,-0.6,-3.53525079574969E-17));
#8666=CARTESIAN_POINT('',(-0.144337567297406,-0.96,-0.25));
#8667=CARTESIAN_POINT('Origin',(-0.144337567297407,-0.6,0.25));
#8668=CARTESIAN_POINT('',(-0.144337567297407,-0.6,0.25));
#8669=CARTESIAN_POINT('',(-0.288675134594813,-0.6,-3.53525079574969E-17));
#8670=CARTESIAN_POINT('',(-0.144337567297407,-0.96,0.25));
#8671=CARTESIAN_POINT('',(-0.144337567297407,-0.6,0.25));
#8672=CARTESIAN_POINT('',(-0.288675134594813,-0.96,-3.53525079574969E-17));
#8673=CARTESIAN_POINT('Origin',(0.144337567297406,-0.6,0.25));
#8674=CARTESIAN_POINT('',(0.144337567297406,-0.6,0.25));
#8675=CARTESIAN_POINT('',(-0.144337567297407,-0.6,0.25));
#8676=CARTESIAN_POINT('',(0.144337567297406,-0.96,0.25));
#8677=CARTESIAN_POINT('',(0.144337567297406,-0.6,0.25));
#8678=CARTESIAN_POINT('',(-0.144337567297407,-0.96,0.25));
#8679=CARTESIAN_POINT('Origin',(0.288675134594813,-0.6,0.));
#8680=CARTESIAN_POINT('',(0.144337567297406,-0.6,0.25));
#8681=CARTESIAN_POINT('',(0.144337567297406,-0.96,0.25));
#8682=CARTESIAN_POINT('Origin',(0.,-0.6,0.));
#8683=CARTESIAN_POINT('Origin',(0.,-0.96,0.));
#8684=CARTESIAN_POINT('',(0.,0.,0.));
#8685=CARTESIAN_POINT('Origin',(0.3,0.4,0.));
#8686=CARTESIAN_POINT('',(-0.3,0.4,-3.67394039744206E-17));
#8687=CARTESIAN_POINT('Origin',(0.,0.4,0.));
#8688=CARTESIAN_POINT('Origin',(0.,0.375,0.));
#8689=CARTESIAN_POINT('',(-0.35,0.35,-4.28626379701573E-17));
#8690=CARTESIAN_POINT('Origin',(0.,0.35,0.));
#8691=CARTESIAN_POINT('',(-0.325,0.375,-3.9801020972289E-17));
#8692=CARTESIAN_POINT('Origin',(0.,0.19,0.));
#8693=CARTESIAN_POINT('',(-0.35,0.03,-4.28626379701574E-17));
#8694=CARTESIAN_POINT('Origin',(0.,0.03,0.));
#8695=CARTESIAN_POINT('',(-0.35,0.19,-4.28626379701574E-17));
#8696=CARTESIAN_POINT('Origin',(0.,0.0149999999999999,0.));
#8697=CARTESIAN_POINT('',(-0.32,-3.29597460435593E-17,-3.91886975727153E-17));
#8698=CARTESIAN_POINT('Origin',(0.,0.,0.));
#8699=CARTESIAN_POINT('',(-0.335,0.0149999999999999,-4.10256677714363E-17));
#8700=CARTESIAN_POINT('Origin',(0.22,0.,0.));
#8701=CARTESIAN_POINT('',(-0.22,-6.93889390390723E-18,-2.69422295812418E-17));
#8702=CARTESIAN_POINT('Origin',(0.,0.,0.));
#8703=CARTESIAN_POINT('Origin',(0.,-0.02,0.));
#8704=CARTESIAN_POINT('',(-0.1954,-0.0492,2.39295984553393E-17));
#8705=CARTESIAN_POINT('Origin',(0.,-0.0492,0.));
#8706=CARTESIAN_POINT('',(-0.21,-0.02,-2.57175827820944E-17));
#8707=CARTESIAN_POINT('Origin',(0.,-0.8,0.));
#8708=CARTESIAN_POINT('',(-0.1954,-1.5646,2.39295984553393E-17));
#8709=CARTESIAN_POINT('Origin',(0.,-1.5646,0.));
#8710=CARTESIAN_POINT('',(-0.1954,-0.8,-2.39295984553393E-17));
#8711=CARTESIAN_POINT('Origin',(0.,-1.58,0.));
#8712=CARTESIAN_POINT('',(-0.16,-1.6,-1.95943487863577E-17));
#8713=CARTESIAN_POINT('Origin',(0.,-1.6,0.));
#8714=CARTESIAN_POINT('',(-0.18,-1.58,-2.20436423846524E-17));
#8715=CARTESIAN_POINT('Origin',(0.,-1.6,0.));
#8716=CARTESIAN_POINT('Origin',(0.0866025403784439,-0.4,-0.15));
#8717=CARTESIAN_POINT('',(0.173205080756888,-0.4,0.));
#8718=CARTESIAN_POINT('',(0.0866025403784439,-0.4,-0.15));
#8719=CARTESIAN_POINT('',(0.173205080756888,-0.4,0.));
#8720=CARTESIAN_POINT('',(0.0866025403784439,-0.64,-0.15));
#8721=CARTESIAN_POINT('',(0.0866025403784439,-0.4,-0.15));
#8722=CARTESIAN_POINT('',(0.173205080756888,-0.64,0.));
#8723=CARTESIAN_POINT('',(0.173205080756888,-0.64,0.));
#8724=CARTESIAN_POINT('',(0.173205080756888,-0.4,0.));
#8725=CARTESIAN_POINT('Origin',(-0.0866025403784438,-0.4,-0.15));
#8726=CARTESIAN_POINT('',(-0.0866025403784438,-0.4,-0.15));
#8727=CARTESIAN_POINT('',(0.0866025403784439,-0.4,-0.15));
#8728=CARTESIAN_POINT('',(-0.0866025403784438,-0.64,-0.15));
#8729=CARTESIAN_POINT('',(-0.0866025403784438,-0.4,-0.15));
#8730=CARTESIAN_POINT('',(0.0866025403784439,-0.64,-0.15));
#8731=CARTESIAN_POINT('Origin',(-0.173205080756888,-0.4,-2.77555756156289E-17));
#8732=CARTESIAN_POINT('',(-0.173205080756888,-0.4,-2.12115047744981E-17));
#8733=CARTESIAN_POINT('',(-0.0866025403784438,-0.4,-0.15));
#8734=CARTESIAN_POINT('',(-0.173205080756888,-0.64,-2.77555756156289E-17));
#8735=CARTESIAN_POINT('',(-0.173205080756888,-0.4,-2.12115047744981E-17));
#8736=CARTESIAN_POINT('',(-0.0866025403784438,-0.64,-0.15));
#8737=CARTESIAN_POINT('Origin',(-0.0866025403784439,-0.4,0.15));
#8738=CARTESIAN_POINT('',(-0.0866025403784439,-0.4,0.15));
#8739=CARTESIAN_POINT('',(-0.173205080756888,-0.4,-2.12115047744981E-17));
#8740=CARTESIAN_POINT('',(-0.0866025403784439,-0.64,0.15));
#8741=CARTESIAN_POINT('',(-0.0866025403784439,-0.4,0.15));
#8742=CARTESIAN_POINT('',(-0.173205080756888,-0.64,-2.12115047744981E-17));
#8743=CARTESIAN_POINT('Origin',(0.0866025403784439,-0.4,0.15));
#8744=CARTESIAN_POINT('',(0.0866025403784439,-0.4,0.15));
#8745=CARTESIAN_POINT('',(-0.0866025403784439,-0.4,0.15));
#8746=CARTESIAN_POINT('',(0.0866025403784439,-0.64,0.15));
#8747=CARTESIAN_POINT('',(0.0866025403784439,-0.4,0.15));
#8748=CARTESIAN_POINT('',(-0.0866025403784439,-0.64,0.15));
#8749=CARTESIAN_POINT('Origin',(0.173205080756888,-0.4,0.));
#8750=CARTESIAN_POINT('',(0.0866025403784439,-0.4,0.15));
#8751=CARTESIAN_POINT('',(0.0866025403784439,-0.64,0.15));
#8752=CARTESIAN_POINT('Origin',(0.,-0.4,-2.77555756156289E-17));
#8753=CARTESIAN_POINT('Origin',(0.,-0.64,-2.77555756156289E-17));
#8754=CARTESIAN_POINT('',(0.,0.,0.));
#8755=CARTESIAN_POINT('',(0.,0.,0.));
#8756=CARTESIAN_POINT('Origin',(0.,8.1,4.5));
#8757=CARTESIAN_POINT('',(-0.21,8.1,4.5));
#8758=CARTESIAN_POINT('Origin',(0.,8.1,4.5));
#8759=CARTESIAN_POINT('',(-0.21,10.,4.5));
#8760=CARTESIAN_POINT('',(-0.21,8.1,4.5));
#8761=CARTESIAN_POINT('Origin',(0.,10.,4.5));
#8762=CARTESIAN_POINT('Origin',(0.,8.1,4.5));
#8763=CARTESIAN_POINT('Origin',(-0.3,8.,3.4));
#8764=CARTESIAN_POINT('',(-0.3,10.,3.54606079858305));
#8765=CARTESIAN_POINT('',(-0.3,8.,3.54606079858305));
#8766=CARTESIAN_POINT('',(-0.3,-4.,3.54606079858305));
#8767=CARTESIAN_POINT('',(-0.3,10.,3.85));
#8768=CARTESIAN_POINT('',(-0.3,10.,3.95));
#8769=CARTESIAN_POINT('',(-0.3,8.,3.85));
#8770=CARTESIAN_POINT('',(-0.3,8.,3.85));
#8771=CARTESIAN_POINT('',(-0.3,8.,3.85));
#8772=CARTESIAN_POINT('Origin',(0.,8.,3.625));
#8773=CARTESIAN_POINT('',(0.3,8.,3.54606079858305));
#8774=CARTESIAN_POINT('Origin',(0.,8.,4.5));
#8775=CARTESIAN_POINT('',(0.3,8.,3.85));
#8776=CARTESIAN_POINT('',(0.3,8.,3.85));
#8777=CARTESIAN_POINT('',(0.3,8.,3.4));
#8778=CARTESIAN_POINT('Origin',(0.3,8.,3.85));
#8779=CARTESIAN_POINT('',(0.3,10.,3.54606079858305));
#8780=CARTESIAN_POINT('',(0.3,-4.,3.54606079858305));
#8781=CARTESIAN_POINT('',(0.3,10.,3.85));
#8782=CARTESIAN_POINT('',(0.3,8.,3.85));
#8783=CARTESIAN_POINT('',(0.3,10.,4.175));
#8784=CARTESIAN_POINT('Origin',(-0.3,8.,3.85));
#8785=CARTESIAN_POINT('',(-0.15,10.,3.85));
#8786=CARTESIAN_POINT('Origin',(0.,-4.,4.5));
#8787=CARTESIAN_POINT('',(-1.,10.,4.5));
#8788=CARTESIAN_POINT('Origin',(0.,10.,4.5));
#8789=CARTESIAN_POINT('',(-1.,0.3,4.5));
#8790=CARTESIAN_POINT('',(-1.,-4.,4.5));
#8791=CARTESIAN_POINT('Origin',(0.,0.3,4.5));
#8792=CARTESIAN_POINT('Origin',(0.,10.,4.5));
#8793=CARTESIAN_POINT('',(0.953939201416946,3.,4.2));
#8794=CARTESIAN_POINT('',(0.953939201416946,3.,4.8));
#8795=CARTESIAN_POINT('Ctrl Pts',(0.953939201416946,3.,4.2));
#8796=CARTESIAN_POINT('Ctrl Pts',(0.953939201416946,2.96207227460108,4.2));
#8797=CARTESIAN_POINT('Ctrl Pts',(0.956437939057488,2.92178925145718,4.20762790839008));
#8798=CARTESIAN_POINT('Ctrl Pts',(0.965284956103208,2.84795244622839,4.23831332738424));
#8799=CARTESIAN_POINT('Ctrl Pts',(0.971486751729016,2.81437646254953,4.26135946873854));
#8800=CARTESIAN_POINT('Ctrl Pts',(0.982993562614982,2.76136736575978,4.31436856552829));
#8801=CARTESIAN_POINT('Ctrl Pts',(0.98907119499008,2.7383151092967,4.34794775809938));
#8802=CARTESIAN_POINT('Ctrl Pts',(0.997630133387832,2.70762517534893,4.42179622825181));
#8803=CARTESIAN_POINT('Ctrl Pts',(1.,2.7,4.4620835734708));
#8804=CARTESIAN_POINT('Ctrl Pts',(1.,2.7,4.5379164265292));
#8805=CARTESIAN_POINT('Ctrl Pts',(0.997630133387832,2.70762517534893,4.57820377174819));
#8806=CARTESIAN_POINT('Ctrl Pts',(0.98907119499008,2.7383151092967,4.65205224190062));
#8807=CARTESIAN_POINT('Ctrl Pts',(0.982993562614982,2.76136736575978,4.68563143447171));
#8808=CARTESIAN_POINT('Ctrl Pts',(0.971486751729016,2.81437646254953,4.73864053126146));
#8809=CARTESIAN_POINT('Ctrl Pts',(0.965284956103208,2.84795244622839,4.76168667261576));
#8810=CARTESIAN_POINT('Ctrl Pts',(0.956437939057488,2.92178925145718,4.79237209160992));
#8811=CARTESIAN_POINT('Ctrl Pts',(0.953939201416946,2.96207227460107,4.8));
#8812=CARTESIAN_POINT('Ctrl Pts',(0.953939201416946,3.,4.8));
#8813=CARTESIAN_POINT('Ctrl Pts',(0.953939201416946,3.,4.8));
#8814=CARTESIAN_POINT('Ctrl Pts',(0.953939201416946,3.03792772539892,4.8));
#8815=CARTESIAN_POINT('Ctrl Pts',(0.956437939057488,3.07821074854282,4.79237209160992));
#8816=CARTESIAN_POINT('Ctrl Pts',(0.965284956103208,3.15204755377161,4.76168667261577));
#8817=CARTESIAN_POINT('Ctrl Pts',(0.971486751729016,3.18562353745047,4.73864053126146));
#8818=CARTESIAN_POINT('Ctrl Pts',(0.982993562614982,3.23863263424022,4.68563143447171));
#8819=CARTESIAN_POINT('Ctrl Pts',(0.98907119499008,3.2616848907033,4.65205224190062));
#8820=CARTESIAN_POINT('Ctrl Pts',(0.997630133387832,3.29237482465107,4.57820377174819));
#8821=CARTESIAN_POINT('Ctrl Pts',(1.,3.3,4.5379164265292));
#8822=CARTESIAN_POINT('Ctrl Pts',(1.,3.3,4.4620835734708));
#8823=CARTESIAN_POINT('Ctrl Pts',(0.997630133387832,3.29237482465107,4.42179622825181));
#8824=CARTESIAN_POINT('Ctrl Pts',(0.98907119499008,3.2616848907033,4.34794775809938));
#8825=CARTESIAN_POINT('Ctrl Pts',(0.982993562614982,3.23863263424022,4.31436856552829));
#8826=CARTESIAN_POINT('Ctrl Pts',(0.971486751729016,3.18562353745047,4.26135946873854));
#8827=CARTESIAN_POINT('Ctrl Pts',(0.965284956103208,3.15204755377161,4.23831332738423));
#8828=CARTESIAN_POINT('Ctrl Pts',(0.956437939057488,3.07821074854282,4.20762790839008));
#8829=CARTESIAN_POINT('Ctrl Pts',(0.953939201416946,3.03792772539892,4.2));
#8830=CARTESIAN_POINT('Ctrl Pts',(0.953939201416946,3.,4.2));
#8831=CARTESIAN_POINT('Origin',(0.,0.3,4.5));
#8832=CARTESIAN_POINT('',(-1.2,0.3,4.5));
#8833=CARTESIAN_POINT('Origin',(0.,0.3,4.5));
#8834=CARTESIAN_POINT('Origin',(0.,0.3,4.5));
#8835=CARTESIAN_POINT('',(-0.4,0.3,4.5));
#8836=CARTESIAN_POINT('Origin',(0.,0.3,4.5));
#8837=CARTESIAN_POINT('Origin',(0.,0.,4.5));
#8838=CARTESIAN_POINT('',(-1.2,0.,4.5));
#8839=CARTESIAN_POINT('Origin',(0.,0.,4.5));
#8840=CARTESIAN_POINT('',(-1.,0.,4.5));
#8841=CARTESIAN_POINT('Origin',(0.,0.,4.5));
#8842=CARTESIAN_POINT('Origin',(0.,0.,4.5));
#8843=CARTESIAN_POINT('',(-0.4,0.,4.5));
#8844=CARTESIAN_POINT('Origin',(0.,0.,4.5));
#8845=CARTESIAN_POINT('Origin',(0.,0.,4.5));
#8846=CARTESIAN_POINT('',(-1.2,0.,4.5));
#8847=CARTESIAN_POINT('Origin',(0.,-4.1,4.5));
#8848=CARTESIAN_POINT('',(-0.4,-2.6,4.5));
#8849=CARTESIAN_POINT('Origin',(0.,-2.6,4.5));
#8850=CARTESIAN_POINT('',(-0.4,-4.1,4.5));
#8851=CARTESIAN_POINT('Origin',(0.,-4.,4.5));
#8852=CARTESIAN_POINT('',(-1.,-4.,4.5));
#8853=CARTESIAN_POINT('',(-1.,-4.,4.5));
#8854=CARTESIAN_POINT('Origin',(0.,-4.,4.5));
#8855=CARTESIAN_POINT('Origin',(0.,-4.1,4.5));
#8856=CARTESIAN_POINT('',(-0.685,-4.,4.5));
#8857=CARTESIAN_POINT('Origin',(0.,-4.,4.5));
#8858=CARTESIAN_POINT('',(-0.685,-2.6,4.5));
#8859=CARTESIAN_POINT('',(-0.685,-4.1,4.5));
#8860=CARTESIAN_POINT('Origin',(0.,-2.6,4.5));
#8861=CARTESIAN_POINT('Origin',(0.,-2.6,4.5));
#8862=CARTESIAN_POINT('Origin',(0.,3.,4.5));
#8863=CARTESIAN_POINT('',(0.264575131106459,3.,4.2));
#8864=CARTESIAN_POINT('',(0.264575131106459,3.,4.8));
#8865=CARTESIAN_POINT('Ctrl Pts',(0.264575131106459,3.,4.2));
#8866=CARTESIAN_POINT('Ctrl Pts',(0.264575131106459,3.02014467721507,4.2));
#8867=CARTESIAN_POINT('Ctrl Pts',(0.266946656583194,3.0403635841556,4.2020492278835));
#8868=CARTESIAN_POINT('Ctrl Pts',(0.275663470560297,3.07974365991683,4.21009513514317));
#8869=CARTESIAN_POINT('Ctrl Pts',(0.281970270384709,3.09891429794725,4.21608711674642));
#8870=CARTESIAN_POINT('Ctrl Pts',(0.304063569802551,3.15349908017058,4.2392312552828));
#8871=CARTESIAN_POINT('Ctrl Pts',(0.322818652826944,3.18607812595988,4.26181405724795));
#8872=CARTESIAN_POINT('Ctrl Pts',(0.35507155223138,3.23763794985389,4.31337388114196));
#8873=CARTESIAN_POINT('Ctrl Pts',(0.371172434841458,3.26054860088286,4.34601764444721));
#8874=CARTESIAN_POINT('Ctrl Pts',(0.393713960479867,3.29176580029427,4.41957074694018));
#8875=CARTESIAN_POINT('Ctrl Pts',(0.4,3.3,4.46055805317426));
#8876=CARTESIAN_POINT('Ctrl Pts',(0.4,3.3,4.53944194682574));
#8877=CARTESIAN_POINT('Ctrl Pts',(0.393713960479867,3.29176580029427,4.58042925305982));
#8878=CARTESIAN_POINT('Ctrl Pts',(0.371172434841458,3.26054860088286,4.65398235555279));
#8879=CARTESIAN_POINT('Ctrl Pts',(0.35507155223138,3.23763794985389,4.68662611885804));
#8880=CARTESIAN_POINT('Ctrl Pts',(0.322818652826944,3.18607812595988,4.73818594275205));
#8881=CARTESIAN_POINT('Ctrl Pts',(0.304063569802551,3.15349908017058,4.7607687447172));
#8882=CARTESIAN_POINT('Ctrl Pts',(0.281970270384709,3.09891429794725,4.78391288325358));
#8883=CARTESIAN_POINT('Ctrl Pts',(0.275663470560297,3.07974365991683,4.78990486485683));
#8884=CARTESIAN_POINT('Ctrl Pts',(0.266946656583194,3.0403635841556,4.7979507721165));
#8885=CARTESIAN_POINT('Ctrl Pts',(0.264575131106459,3.02014467721507,4.8));
#8886=CARTESIAN_POINT('Ctrl Pts',(0.264575131106459,3.,4.8));
#8887=CARTESIAN_POINT('Ctrl Pts',(0.264575131106459,3.,4.8));
#8888=CARTESIAN_POINT('Ctrl Pts',(0.264575131106459,2.97985532278493,4.8));
#8889=CARTESIAN_POINT('Ctrl Pts',(0.266946656583194,2.9596364158444,4.7979507721165));
#8890=CARTESIAN_POINT('Ctrl Pts',(0.275663470560297,2.92025634008317,4.78990486485683));
#8891=CARTESIAN_POINT('Ctrl Pts',(0.281970270384709,2.90108570205275,4.78391288325358));
#8892=CARTESIAN_POINT('Ctrl Pts',(0.304063569802551,2.84650091982942,4.7607687447172));
#8893=CARTESIAN_POINT('Ctrl Pts',(0.322818652826944,2.81392187404012,4.73818594275205));
#8894=CARTESIAN_POINT('Ctrl Pts',(0.35507155223138,2.76236205014611,4.68662611885804));
#8895=CARTESIAN_POINT('Ctrl Pts',(0.371172434841458,2.73945139911714,4.65398235555279));
#8896=CARTESIAN_POINT('Ctrl Pts',(0.393713960479867,2.70823419970573,4.58042925305983));
#8897=CARTESIAN_POINT('Ctrl Pts',(0.4,2.7,4.53944194682573));
#8898=CARTESIAN_POINT('Ctrl Pts',(0.4,2.7,4.46055805317426));
#8899=CARTESIAN_POINT('Ctrl Pts',(0.393713960479867,2.70823419970573,4.41957074694017));
#8900=CARTESIAN_POINT('Ctrl Pts',(0.371172434841458,2.73945139911714,4.34601764444721));
#8901=CARTESIAN_POINT('Ctrl Pts',(0.35507155223138,2.76236205014611,4.31337388114196));
#8902=CARTESIAN_POINT('Ctrl Pts',(0.322818652826944,2.81392187404012,4.26181405724795));
#8903=CARTESIAN_POINT('Ctrl Pts',(0.304063569802551,2.84650091982942,4.2392312552828));
#8904=CARTESIAN_POINT('Ctrl Pts',(0.281970270384709,2.90108570205275,4.21608711674642));
#8905=CARTESIAN_POINT('Ctrl Pts',(0.275663470560297,2.92025634008317,4.21009513514317));
#8906=CARTESIAN_POINT('Ctrl Pts',(0.266946656583194,2.9596364158444,4.2020492278835));
#8907=CARTESIAN_POINT('Ctrl Pts',(0.264575131106459,2.97985532278493,4.2));
#8908=CARTESIAN_POINT('Ctrl Pts',(0.264575131106459,3.,4.2));
#8909=CARTESIAN_POINT('',(0.,3.,4.8));
#8910=CARTESIAN_POINT('Origin',(0.,-4.1,4.5));
#8911=CARTESIAN_POINT('',(-0.4,6.5,4.5));
#8912=CARTESIAN_POINT('',(-0.4,-4.1,4.5));
#8913=CARTESIAN_POINT('Origin',(0.,6.5,4.5));
#8914=CARTESIAN_POINT('Origin',(0.,6.5,4.5));
#8915=CARTESIAN_POINT('Origin',(0.,10.,4.5));
#8916=CARTESIAN_POINT('Origin',(0.,-4.,4.5));
#8917=CARTESIAN_POINT('',(0.,0.,0.));
#8918=CARTESIAN_POINT('Origin',(0.,5.7,4.5));
#8919=CARTESIAN_POINT('',(-1.005,6.4,4.5));
#8920=CARTESIAN_POINT('Origin',(0.,6.4,4.5));
#8921=CARTESIAN_POINT('',(-1.005,5.7,4.5));
#8922=CARTESIAN_POINT('',(-1.005,5.7,4.5));
#8923=CARTESIAN_POINT('Origin',(0.,5.7,4.5));
#8924=CARTESIAN_POINT('Origin',(0.,5.7,4.5));
#8925=CARTESIAN_POINT('',(-1.35,6.4,4.5));
#8926=CARTESIAN_POINT('Origin',(0.,6.4,4.5));
#8927=CARTESIAN_POINT('',(-1.35,5.7,4.5));
#8928=CARTESIAN_POINT('',(-1.35,5.7,4.5));
#8929=CARTESIAN_POINT('Origin',(0.,5.7,4.5));
#8930=CARTESIAN_POINT('Origin',(0.,6.4,4.5));
#8931=CARTESIAN_POINT('Origin',(0.,5.7,4.5));
#8932=CARTESIAN_POINT('',(0.,0.,0.));
#8933=CARTESIAN_POINT('Origin',(0.,6.8,5.49));
#8934=CARTESIAN_POINT('',(0.172988438920061,6.68094119100209,5.49));
#8935=CARTESIAN_POINT('',(0.172988438920061,6.91905880899791,5.49));
#8936=CARTESIAN_POINT('',(0.172988438920061,6.4,5.49));
#8937=CARTESIAN_POINT('Origin',(0.,6.8,5.49));
#8938=CARTESIAN_POINT('Origin',(0.,6.8,5.49));
#8939=CARTESIAN_POINT('',(-0.172988438920061,6.68094119100209,5.49));
#8940=CARTESIAN_POINT('Ctrl Pts',(-0.172988438920061,6.68094119100209,5.49));
#8941=CARTESIAN_POINT('Ctrl Pts',(-0.165594865311318,6.67019857760471,5.49129192197638));
#8942=CARTESIAN_POINT('Ctrl Pts',(-0.157297138725608,6.66031229062726,5.49265394943905));
#8943=CARTESIAN_POINT('Ctrl Pts',(-0.129892073845076,6.63290722574673,5.4967480843909));
#8944=CARTESIAN_POINT('Ctrl Pts',(-0.106330167759285,6.61675794366705,5.49969589327638));
#8945=CARTESIAN_POINT('Ctrl Pts',(-0.0546129046324107,6.59530220603509,
5.50385029472357));
#8946=CARTESIAN_POINT('Ctrl Pts',(-0.0264512308298516,6.59,5.505));
#8947=CARTESIAN_POINT('Ctrl Pts',(0.0264512308298515,6.59,5.505));
#8948=CARTESIAN_POINT('Ctrl Pts',(0.0546129046324106,6.59530220603509,5.50385029472357));
#8949=CARTESIAN_POINT('Ctrl Pts',(0.106330167759285,6.61675794366705,5.49969589327638));
#8950=CARTESIAN_POINT('Ctrl Pts',(0.129892073845076,6.63290722574673,5.4967480843909));
#8951=CARTESIAN_POINT('Ctrl Pts',(0.157297138725608,6.66031229062726,5.49265394943905));
#8952=CARTESIAN_POINT('Ctrl Pts',(0.165594865311318,6.67019857760471,5.49129192197638));
#8953=CARTESIAN_POINT('Ctrl Pts',(0.172988438920061,6.68094119100209,5.49));
#8954=CARTESIAN_POINT('',(-0.21,6.8,5.49));
#8955=CARTESIAN_POINT('Origin',(0.,6.8,5.49));
#8956=CARTESIAN_POINT('',(-0.21,6.8,5.98522725533839));
#8957=CARTESIAN_POINT('',(-0.21,6.8,5.49));
#8958=CARTESIAN_POINT('',(0.21,6.8,5.98522725533839));
#8959=CARTESIAN_POINT('Ctrl Pts',(0.21,6.8,5.98522725533839));
#8960=CARTESIAN_POINT('Ctrl Pts',(0.21,6.77359447307555,5.98522725533839));
#8961=CARTESIAN_POINT('Ctrl Pts',(0.204715737269596,6.74545292590929,5.98600415954412));
#8962=CARTESIAN_POINT('Ctrl Pts',(0.183273763036331,6.69372373109487,5.98880073282317));
#8963=CARTESIAN_POINT('Ctrl Pts',(0.167117923970394,6.67013307587204,5.99077897157582));
#8964=CARTESIAN_POINT('Ctrl Pts',(0.129867169887369,6.63288232178902,5.99448481141327));
#8965=CARTESIAN_POINT('Ctrl Pts',(0.106276408305765,6.61672628999865,5.99645455657129));
#8966=CARTESIAN_POINT('Ctrl Pts',(0.0545468514059003,6.59528417517378,5.99923165515646));
#8967=CARTESIAN_POINT('Ctrl Pts',(0.0264051785092814,6.59,6.));
#8968=CARTESIAN_POINT('Ctrl Pts',(-0.0264051785092814,6.59,6.));
#8969=CARTESIAN_POINT('Ctrl Pts',(-0.0545468514059002,6.59528417517378,
5.99923165515646));
#8970=CARTESIAN_POINT('Ctrl Pts',(-0.106276408305765,6.61672628999865,5.99645455657129));
#8971=CARTESIAN_POINT('Ctrl Pts',(-0.129867169887369,6.63288232178902,5.99448481141327));
#8972=CARTESIAN_POINT('Ctrl Pts',(-0.167117923970394,6.67013307587204,5.99077897157582));
#8973=CARTESIAN_POINT('Ctrl Pts',(-0.183273763036331,6.69372373109487,5.98880073282317));
#8974=CARTESIAN_POINT('Ctrl Pts',(-0.204715737269596,6.74545292590929,5.98600415954412));
#8975=CARTESIAN_POINT('Ctrl Pts',(-0.21,6.77359447307555,5.98522725533839));
#8976=CARTESIAN_POINT('Ctrl Pts',(-0.21,6.8,5.98522725533839));
#8977=CARTESIAN_POINT('Ctrl Pts',(-0.21,6.8,5.98522725533839));
#8978=CARTESIAN_POINT('Ctrl Pts',(-0.21,6.82640552692445,5.98522725533839));
#8979=CARTESIAN_POINT('Ctrl Pts',(-0.204715737269596,6.85454707409071,5.98600415954412));
#8980=CARTESIAN_POINT('Ctrl Pts',(-0.183273763036331,6.90627626890513,5.98880073282317));
#8981=CARTESIAN_POINT('Ctrl Pts',(-0.167117923970394,6.92986692412796,5.99077897157582));
#8982=CARTESIAN_POINT('Ctrl Pts',(-0.129867169887369,6.96711767821098,5.99448481141327));
#8983=CARTESIAN_POINT('Ctrl Pts',(-0.106276408305765,6.98327371000135,5.99645455657129));
#8984=CARTESIAN_POINT('Ctrl Pts',(-0.0545468514059003,7.00471582482622,
5.99923165515646));
#8985=CARTESIAN_POINT('Ctrl Pts',(-0.0264051785092815,7.01,6.));
#8986=CARTESIAN_POINT('Ctrl Pts',(0.0264051785092814,7.01,6.));
#8987=CARTESIAN_POINT('Ctrl Pts',(0.0545468514058999,7.00471582482622,5.99923165515646));
#8988=CARTESIAN_POINT('Ctrl Pts',(0.106276408305765,6.98327371000135,5.99645455657129));
#8989=CARTESIAN_POINT('Ctrl Pts',(0.129867169887369,6.96711767821098,5.99448481141327));
#8990=CARTESIAN_POINT('Ctrl Pts',(0.167117923970393,6.92986692412796,5.99077897157582));
#8991=CARTESIAN_POINT('Ctrl Pts',(0.183273763036332,6.90627626890513,5.98880073282317));
#8992=CARTESIAN_POINT('Ctrl Pts',(0.204715737269596,6.85454707409071,5.98600415954412));
#8993=CARTESIAN_POINT('Ctrl Pts',(0.21,6.82640552692445,5.98522725533839));
#8994=CARTESIAN_POINT('Ctrl Pts',(0.21,6.8,5.98522725533839));
#8995=CARTESIAN_POINT('',(-0.172988438920061,6.91905880899791,5.49));
#8996=CARTESIAN_POINT('Origin',(0.,6.8,5.49));
#8997=CARTESIAN_POINT('Ctrl Pts',(0.172988438920062,6.91905880899791,5.49));
#8998=CARTESIAN_POINT('Ctrl Pts',(0.165594865311319,6.92980142239529,5.49129192197638));
#8999=CARTESIAN_POINT('Ctrl Pts',(0.157297138725609,6.93968770937274,5.49265394943905));
#9000=CARTESIAN_POINT('Ctrl Pts',(0.129892073845076,6.96709277425327,5.4967480843909));
#9001=CARTESIAN_POINT('Ctrl Pts',(0.106330167759285,6.98324205633295,5.49969589327638));
#9002=CARTESIAN_POINT('Ctrl Pts',(0.0546129046324107,7.00469779396491,5.50385029472357));
#9003=CARTESIAN_POINT('Ctrl Pts',(0.0264512308298516,7.01,5.505));
#9004=CARTESIAN_POINT('Ctrl Pts',(-0.0264512308298515,7.01,5.505));
#9005=CARTESIAN_POINT('Ctrl Pts',(-0.0546129046324097,7.00469779396491,
5.50385029472357));
#9006=CARTESIAN_POINT('Ctrl Pts',(-0.106330167759284,6.98324205633295,5.49969589327638));
#9007=CARTESIAN_POINT('Ctrl Pts',(-0.129892073845076,6.96709277425327,5.4967480843909));
#9008=CARTESIAN_POINT('Ctrl Pts',(-0.157297138725609,6.93968770937274,5.49265394943905));
#9009=CARTESIAN_POINT('Ctrl Pts',(-0.165594865311318,6.92980142239529,5.49129192197638));
#9010=CARTESIAN_POINT('Ctrl Pts',(-0.172988438920061,6.91905880899791,5.49));
#9011=CARTESIAN_POINT('Origin',(0.,6.8,5.49));
#9012=CARTESIAN_POINT('',(-0.172988438920061,6.4,5.49));
#9013=CARTESIAN_POINT('Origin',(0.,6.4,4.5));
#9014=CARTESIAN_POINT('',(-1.005,7.2,4.5));
#9015=CARTESIAN_POINT('Origin',(0.,7.2,4.5));
#9016=CARTESIAN_POINT('',(-1.005,6.4,4.5));
#9017=CARTESIAN_POINT('',(-1.005,6.4,4.5));
#9018=CARTESIAN_POINT('Origin',(0.,6.4,4.5));
#9019=CARTESIAN_POINT('Origin',(0.,6.4,4.5));
#9020=CARTESIAN_POINT('',(-1.5,7.2,4.5));
#9021=CARTESIAN_POINT('Origin',(0.,7.2,4.5));
#9022=CARTESIAN_POINT('',(-1.5,6.4,4.5));
#9023=CARTESIAN_POINT('',(-1.5,6.4,4.5));
#9024=CARTESIAN_POINT('Origin',(0.,6.4,4.5));
#9025=CARTESIAN_POINT('Origin',(0.,7.2,4.5));
#9026=CARTESIAN_POINT('Origin',(0.,6.4,4.5));
#9027=CARTESIAN_POINT('',(0.,0.,0.));
#9028=CARTESIAN_POINT('Origin',(-0.3,7.7,3.22));
#9029=CARTESIAN_POINT('',(-0.3,7.8,3.22));
#9030=CARTESIAN_POINT('',(-0.3,7.8,3.54606079858305));
#9031=CARTESIAN_POINT('',(-0.3,7.8,3.86));
#9032=CARTESIAN_POINT('',(-0.3,10.,3.22));
#9033=CARTESIAN_POINT('',(-0.3,7.7,3.22));
#9034=CARTESIAN_POINT('',(-0.3,10.,3.54606079858305));
#9035=CARTESIAN_POINT('',(-0.3,10.,3.86));
#9036=CARTESIAN_POINT('',(-0.3,7.8,3.54606079858305));
#9037=CARTESIAN_POINT('Origin',(0.3,7.7,3.22));
#9038=CARTESIAN_POINT('',(0.3,7.8,3.22));
#9039=CARTESIAN_POINT('',(0.15,7.8,3.22));
#9040=CARTESIAN_POINT('',(0.3,10.,3.22));
#9041=CARTESIAN_POINT('',(0.3,7.7,3.22));
#9042=CARTESIAN_POINT('',(0.15,10.,3.22));
#9043=CARTESIAN_POINT('Origin',(0.3,7.7,4.5));
#9044=CARTESIAN_POINT('',(0.3,7.8,3.54606079858305));
#9045=CARTESIAN_POINT('',(0.3,7.8,4.5));
#9046=CARTESIAN_POINT('',(0.3,10.,3.54606079858305));
#9047=CARTESIAN_POINT('',(0.3,7.8,3.54606079858305));
#9048=CARTESIAN_POINT('',(0.3,10.,4.5));
#9049=CARTESIAN_POINT('Origin',(0.,10.,4.5));
#9050=CARTESIAN_POINT('',(-3.,10.,4.5));
#9051=CARTESIAN_POINT('Origin',(0.,10.,4.5));
#9052=CARTESIAN_POINT('',(-2.675,10.,4.5));
#9053=CARTESIAN_POINT('Origin',(-2.4,10.,4.5));
#9054=CARTESIAN_POINT('',(-0.275,10.,6.9));
#9055=CARTESIAN_POINT('Origin',(1.46957615897682E-16,10.,6.9));
#9056=CARTESIAN_POINT('',(2.125,10.,4.5));
#9057=CARTESIAN_POINT('Origin',(2.4,10.,4.5));
#9058=CARTESIAN_POINT('',(-0.275,10.,2.1));
#9059=CARTESIAN_POINT('Origin',(-4.40872847693047E-16,10.,2.1));
#9060=CARTESIAN_POINT('Origin',(0.,10.,4.5));
#9061=CARTESIAN_POINT('Origin',(0.,7.8,4.5));
#9062=CARTESIAN_POINT('Origin',(0.,7.8,4.5));
#9063=CARTESIAN_POINT('Origin',(-2.4,9.4,4.5));
#9064=CARTESIAN_POINT('',(-2.675,9.5,4.5));
#9065=CARTESIAN_POINT('Origin',(-2.4,9.5,4.5));
#9066=CARTESIAN_POINT('',(-2.675,9.4,4.5));
#9067=CARTESIAN_POINT('Origin',(1.46957615897682E-16,9.4,6.9));
#9068=CARTESIAN_POINT('',(-0.275,9.5,6.9));
#9069=CARTESIAN_POINT('Origin',(1.46957615897682E-16,9.5,6.9));
#9070=CARTESIAN_POINT('',(-0.275,9.4,6.9));
#9071=CARTESIAN_POINT('Origin',(2.4,9.4,4.5));
#9072=CARTESIAN_POINT('',(2.125,9.5,4.5));
#9073=CARTESIAN_POINT('Origin',(2.4,9.5,4.5));
#9074=CARTESIAN_POINT('',(2.125,9.4,4.5));
#9075=CARTESIAN_POINT('Origin',(-4.40872847693047E-16,9.4,2.1));
#9076=CARTESIAN_POINT('',(-0.275,9.5,2.1));
#9077=CARTESIAN_POINT('Origin',(-4.40872847693047E-16,9.5,2.1));
#9078=CARTESIAN_POINT('',(-0.275,9.4,2.1));
#9079=CARTESIAN_POINT('Origin',(0.,9.5,4.5));
#9080=CARTESIAN_POINT('',(-3.,9.5,4.5));
#9081=CARTESIAN_POINT('Origin',(0.,9.5,4.5));
#9082=CARTESIAN_POINT('',(-1.6,9.5,4.5));
#9083=CARTESIAN_POINT('Origin',(0.,9.5,4.5));
#9084=CARTESIAN_POINT('Origin',(0.,9.5,4.5));
#9085=CARTESIAN_POINT('',(-3.,9.5,4.5));
#9086=CARTESIAN_POINT('Origin',(0.,7.8,4.5));
#9087=CARTESIAN_POINT('',(-1.6,7.8,4.5));
#9088=CARTESIAN_POINT('',(-1.6,7.8,4.5));
#9089=CARTESIAN_POINT('Origin',(0.,7.8,4.5));
#9090=CARTESIAN_POINT('Origin',(0.,7.8,4.5));
#9091=CARTESIAN_POINT('',(0.,0.,0.));
#9092=CARTESIAN_POINT('Origin',(0.,10.,4.5));
#9093=CARTESIAN_POINT('',(-0.275,10.2,4.5));
#9094=CARTESIAN_POINT('Origin',(0.,10.2,4.5));
#9095=CARTESIAN_POINT('',(-0.275,10.,4.5));
#9096=CARTESIAN_POINT('',(-0.275,10.,4.5));
#9097=CARTESIAN_POINT('Origin',(0.,10.,4.5));
#9098=CARTESIAN_POINT('Origin',(0.,10.,4.5));
#9099=CARTESIAN_POINT('',(-1.2,10.2,4.5));
#9100=CARTESIAN_POINT('Origin',(0.,10.2,4.5));
#9101=CARTESIAN_POINT('',(-1.2,10.,4.5));
#9102=CARTESIAN_POINT('',(-1.2,10.,4.5));
#9103=CARTESIAN_POINT('Origin',(0.,10.,4.5));
#9104=CARTESIAN_POINT('Origin',(0.,10.2,4.5));
#9105=CARTESIAN_POINT('Origin',(0.,10.,4.5));
#9106=CARTESIAN_POINT('',(0.,0.,0.));
#9107=CARTESIAN_POINT('Origin',(0.,-0.4,0.));
#9108=CARTESIAN_POINT('',(1.01036297108185,-0.4,0.));
#9109=CARTESIAN_POINT('',(0.505181485540923,-0.4,0.875));
#9110=CARTESIAN_POINT('',(0.505181485540923,-0.4,0.875));
#9111=CARTESIAN_POINT('',(-0.505181485540923,-0.4,0.875));
#9112=CARTESIAN_POINT('',(-0.505181485540923,-0.4,0.875));
#9113=CARTESIAN_POINT('',(-1.01036297108185,-0.4,-1.23733777851239E-16));
#9114=CARTESIAN_POINT('',(-1.01036297108185,-0.4,-1.23733777851239E-16));
#9115=CARTESIAN_POINT('',(-0.505181485540922,-0.4,-0.875));
#9116=CARTESIAN_POINT('',(-0.505181485540922,-0.4,-0.875));
#9117=CARTESIAN_POINT('',(0.505181485540923,-0.4,-0.875));
#9118=CARTESIAN_POINT('',(0.505181485540923,-0.4,-0.875));
#9119=CARTESIAN_POINT('',(1.01036297108185,-0.4,0.));
#9120=CARTESIAN_POINT('',(-0.685,-0.4,-8.38883057415937E-17));
#9121=CARTESIAN_POINT('Origin',(0.,-0.4,0.));
#9122=CARTESIAN_POINT('Origin',(0.,0.4,0.));
#9123=CARTESIAN_POINT('',(0.505181485540923,0.4,0.875));
#9124=CARTESIAN_POINT('',(1.01036297108185,0.4,0.));
#9125=CARTESIAN_POINT('',(0.505181485540923,0.4,0.875));
#9126=CARTESIAN_POINT('',(0.505181485540923,0.4,-0.875));
#9127=CARTESIAN_POINT('',(1.01036297108185,0.4,0.));
#9128=CARTESIAN_POINT('',(-0.505181485540922,0.4,-0.875));
#9129=CARTESIAN_POINT('',(0.505181485540923,0.4,-0.875));
#9130=CARTESIAN_POINT('',(-1.01036297108185,0.4,-1.23733777851239E-16));
#9131=CARTESIAN_POINT('',(-0.505181485540922,0.4,-0.875));
#9132=CARTESIAN_POINT('',(-0.505181485540923,0.4,0.875));
#9133=CARTESIAN_POINT('',(-1.01036297108185,0.4,-1.23733777851239E-16));
#9134=CARTESIAN_POINT('',(-0.505181485540923,0.4,0.875));
#9135=CARTESIAN_POINT('',(-0.685,0.4,8.38883057415937E-17));
#9136=CARTESIAN_POINT('Origin',(0.,0.4,0.));
#9137=CARTESIAN_POINT('Origin',(-0.505181485540923,0.,0.875));
#9138=CARTESIAN_POINT('',(0.505181485540923,0.,0.875));
#9139=CARTESIAN_POINT('',(-0.505181485540923,0.,0.875));
#9140=CARTESIAN_POINT('Origin',(-1.01036297108185,0.,-1.23733777851239E-16));
#9141=CARTESIAN_POINT('',(-1.01036297108185,0.,-1.23733777851239E-16));
#9142=CARTESIAN_POINT('Origin',(-0.505181485540922,0.,-0.875));
#9143=CARTESIAN_POINT('',(-0.505181485540922,0.,-0.875));
#9144=CARTESIAN_POINT('Origin',(0.505181485540923,0.,-0.875));
#9145=CARTESIAN_POINT('',(0.505181485540923,0.,-0.875));
#9146=CARTESIAN_POINT('Origin',(1.01036297108185,0.,0.));
#9147=CARTESIAN_POINT('',(1.01036297108185,0.,0.));
#9148=CARTESIAN_POINT('Origin',(0.505181485540923,0.,0.875));
#9149=CARTESIAN_POINT('Origin',(0.,0.,0.));
#9150=CARTESIAN_POINT('',(-0.685,1.82,-8.38883057415937E-17));
#9151=CARTESIAN_POINT('',(-0.685,0.,-8.38883057415937E-17));
#9152=CARTESIAN_POINT('Origin',(0.,1.82,0.));
#9153=CARTESIAN_POINT('Origin',(0.605,1.9,0.));
#9154=CARTESIAN_POINT('',(-0.605,1.9,-7.40911313484149E-17));
#9155=CARTESIAN_POINT('Origin',(0.,1.9,0.));
#9156=CARTESIAN_POINT('',(-0.46,1.9,-5.63337527607782E-17));
#9157=CARTESIAN_POINT('Origin',(0.,1.9,0.));
#9158=CARTESIAN_POINT('Origin',(0.,1.86,0.));
#9159=CARTESIAN_POINT('',(-0.645,1.86,-7.89897185450043E-17));
#9160=CARTESIAN_POINT('Origin',(0.,0.,0.));
#9161=CARTESIAN_POINT('',(-0.685,-1.82,-8.38883057415937E-17));
#9162=CARTESIAN_POINT('Origin',(0.,-1.82,0.));
#9163=CARTESIAN_POINT('',(-0.685,0.,-8.38883057415937E-17));
#9164=CARTESIAN_POINT('Origin',(0.,-1.86,0.));
#9165=CARTESIAN_POINT('',(-0.605,-1.9,-7.40911313484149E-17));
#9166=CARTESIAN_POINT('Origin',(0.,-1.9,0.));
#9167=CARTESIAN_POINT('',(-0.645,-1.86,-7.89897185450043E-17));
#9168=CARTESIAN_POINT('Origin',(0.46,-1.9,0.));
#9169=CARTESIAN_POINT('',(-0.46,-1.9,-5.63337527607782E-17));
#9170=CARTESIAN_POINT('Origin',(0.,-1.9,0.));
#9171=CARTESIAN_POINT('Origin',(0.,0.,0.));
#9172=CARTESIAN_POINT('',(-0.46,0.,-5.63337527607782E-17));
#9173=CARTESIAN_POINT('',(0.,0.,0.));
#9174=CARTESIAN_POINT('',(0.,0.,0.));
#9175=CARTESIAN_POINT('',(0.,0.,0.));
#9176=CARTESIAN_POINT('',(0.,0.,0.));
#9177=CARTESIAN_POINT('',(0.,0.,0.));
#9178=CARTESIAN_POINT('',(0.,0.,0.));
#9179=CARTESIAN_POINT('',(0.,0.,0.));
#9180=CARTESIAN_POINT('',(0.,0.,0.));
#9181=CARTESIAN_POINT('',(0.,0.,0.));
#9182=CARTESIAN_POINT('',(0.,0.,0.));
#9183=CARTESIAN_POINT('',(0.,0.,0.));
#9184=CARTESIAN_POINT('',(0.,1.,4.5));
#9185=CARTESIAN_POINT('',(-3.8,1.,2.5));
#9186=CARTESIAN_POINT('',(3.8,1.,2.5));
#9187=CARTESIAN_POINT('',(0.,5.,4.5));
#9188=CARTESIAN_POINT('',(-3.8,5.,2.5));
#9189=CARTESIAN_POINT('',(3.8,5.,2.5));
#9190=CARTESIAN_POINT('',(4.3,3.,4.5));
#9191=CARTESIAN_POINT('',(2.8,-0.4,4.5));
#9192=CARTESIAN_POINT('',(0.,-0.4,7.3));
#9193=CARTESIAN_POINT('',(-2.8,-0.4,4.5));
#9194=CARTESIAN_POINT('',(-4.44089209850063E-16,-0.4,1.7));
#9195=CARTESIAN_POINT('',(2.8,6.4,4.5));
#9196=CARTESIAN_POINT('',(4.44089209850063E-16,6.4,7.3));
#9197=CARTESIAN_POINT('',(-2.8,6.4,4.5));
#9198=CARTESIAN_POINT('',(-4.44089209850063E-16,6.4,1.7));
#9199=CARTESIAN_POINT('',(0.,0.,0.));
#9200=CARTESIAN_POINT('Origin',(0.0721687836487032,0.,-0.125));
#9201=CARTESIAN_POINT('',(0.0721687836487032,0.,-0.125));
#9202=CARTESIAN_POINT('',(0.144337567297406,0.,0.));
#9203=CARTESIAN_POINT('',(0.117710979560879,0.,-0.0461186027918559));
#9204=CARTESIAN_POINT('',(0.0721687836487032,-0.25,-0.125));
#9205=CARTESIAN_POINT('',(0.0721687836487032,0.,-0.125));
#9206=CARTESIAN_POINT('',(0.144337567297406,-0.25,0.));
#9207=CARTESIAN_POINT('',(0.144337567297406,-0.25,0.));
#9208=CARTESIAN_POINT('',(0.144337567297406,0.,0.));
#9209=CARTESIAN_POINT('Origin',(-0.0721687836487032,0.,-0.125));
#9210=CARTESIAN_POINT('',(-0.0721687836487032,0.,-0.125));
#9211=CARTESIAN_POINT('',(0.0739156081756484,0.,-0.125));
#9212=CARTESIAN_POINT('',(-0.0721687836487032,-0.25,-0.125));
#9213=CARTESIAN_POINT('',(-0.0721687836487032,0.,-0.125));
#9214=CARTESIAN_POINT('',(0.0721687836487032,-0.25,-0.125));
#9215=CARTESIAN_POINT('Origin',(-0.144337567297406,0.,-4.16333634234434E-17));
#9216=CARTESIAN_POINT('',(-0.144337567297406,0.,-1.76762539787485E-17));
#9217=CARTESIAN_POINT('',(-0.0987953713852306,0.,-0.0788813972081442));
#9218=CARTESIAN_POINT('',(-0.144337567297406,-0.25,-2.77555756156289E-17));
#9219=CARTESIAN_POINT('',(-0.144337567297406,0.,-1.76762539787485E-17));
#9220=CARTESIAN_POINT('',(-0.0721687836487032,-0.25,-0.125));
#9221=CARTESIAN_POINT('Origin',(-0.0721687836487033,0.,0.125));
#9222=CARTESIAN_POINT('',(-0.0721687836487033,0.,0.125));
#9223=CARTESIAN_POINT('',(-0.0627109795608791,0.,0.141381397208144));
#9224=CARTESIAN_POINT('',(-0.0721687836487033,-0.25,0.125));
#9225=CARTESIAN_POINT('',(-0.0721687836487033,0.,0.125));
#9226=CARTESIAN_POINT('',(-0.144337567297406,-0.25,-1.76762539787485E-17));
#9227=CARTESIAN_POINT('Origin',(0.0721687836487032,0.,0.125));
#9228=CARTESIAN_POINT('',(0.0721687836487032,0.,0.125));
#9229=CARTESIAN_POINT('',(0.146084391824352,0.,0.125));
#9230=CARTESIAN_POINT('',(0.0721687836487032,-0.25,0.125));
#9231=CARTESIAN_POINT('',(0.0721687836487032,0.,0.125));
#9232=CARTESIAN_POINT('',(-0.0721687836487033,-0.25,0.125));
#9233=CARTESIAN_POINT('Origin',(0.144337567297406,0.,0.));
#9234=CARTESIAN_POINT('',(0.153795371385231,0.,-0.0163813972081441));
#9235=CARTESIAN_POINT('',(0.0721687836487032,-0.25,0.125));
#9236=CARTESIAN_POINT('Origin',(0.,-0.25,0.));
#9237=CARTESIAN_POINT('Origin',(0.22,0.,0.));
#9238=CARTESIAN_POINT('',(-0.22,-8.67361737988404E-18,-2.69422295812418E-17));
#9239=CARTESIAN_POINT('Origin',(0.,0.,0.));
#9240=CARTESIAN_POINT('Origin',(0.,-0.015,0.));
#9241=CARTESIAN_POINT('',(-0.24505,-0.02505,-3.00099698131059E-17));
#9242=CARTESIAN_POINT('Origin',(0.,-0.02505,0.));
#9243=CARTESIAN_POINT('',(-0.235,-0.015,-2.87791997799628E-17));
#9244=CARTESIAN_POINT('Origin',(0.,-0.3775,0.));
#9245=CARTESIAN_POINT('',(-0.24505,-0.72995,3.00099698131059E-17));
#9246=CARTESIAN_POINT('Origin',(0.,-0.72995,0.));
#9247=CARTESIAN_POINT('',(-0.24505,-0.3775,-3.00099698131059E-17));
#9248=CARTESIAN_POINT('Origin',(0.,-0.7625,0.));
#9249=CARTESIAN_POINT('',(-0.175,-0.8,-2.14313189850787E-17));
#9250=CARTESIAN_POINT('Origin',(0.,-0.8,0.));
#9251=CARTESIAN_POINT('',(-0.2125,-0.7625,-2.60237444818813E-17));
#9252=CARTESIAN_POINT('Origin',(0.,-0.8,0.));
#9253=CARTESIAN_POINT('',(0.,0.,0.));
#9254=CARTESIAN_POINT('Origin',(-1.,0.,0.35));
#9255=CARTESIAN_POINT('',(-1.,-0.26,0.6));
#9256=CARTESIAN_POINT('',(-1.,-0.3,0.56));
#9257=CARTESIAN_POINT('',(-1.,-0.2675,0.5925));
#9258=CARTESIAN_POINT('',(-1.,0.26,0.6));
#9259=CARTESIAN_POINT('',(-1.,0.,0.6));
#9260=CARTESIAN_POINT('',(-1.,0.3,0.56));
#9261=CARTESIAN_POINT('',(-1.,0.2675,0.5925));
#9262=CARTESIAN_POINT('',(-1.,0.3,0.04));
#9263=CARTESIAN_POINT('',(-1.,0.3,0.175));
#9264=CARTESIAN_POINT('',(-1.,0.26,0.));
#9265=CARTESIAN_POINT('',(-1.,0.2925,0.0325));
#9266=CARTESIAN_POINT('',(-1.,-0.26,0.));
#9267=CARTESIAN_POINT('',(-1.,0.,0.));
#9268=CARTESIAN_POINT('',(-1.,-0.3,0.04));
#9269=CARTESIAN_POINT('',(-1.,-0.2925,0.0325));
#9270=CARTESIAN_POINT('',(-1.,-0.3,0.175));
#9271=CARTESIAN_POINT('Origin',(0.75,0.28,0.02));
#9272=CARTESIAN_POINT('',(1.,0.3,0.04));
#9273=CARTESIAN_POINT('',(0.75,0.3,0.04));
#9274=CARTESIAN_POINT('',(1.,0.26,0.));
#9275=CARTESIAN_POINT('',(1.,0.2925,0.0325));
#9276=CARTESIAN_POINT('',(0.75,0.26,0.));
#9277=CARTESIAN_POINT('Origin',(1.5,0.3,0.));
#9278=CARTESIAN_POINT('',(1.,0.3,0.56));
#9279=CARTESIAN_POINT('',(0.75,0.3,0.56));
#9280=CARTESIAN_POINT('',(1.,0.3,0.175));
#9281=CARTESIAN_POINT('Origin',(0.75,0.28,0.58));
#9282=CARTESIAN_POINT('',(1.,0.26,0.6));
#9283=CARTESIAN_POINT('',(0.75,0.26,0.6));
#9284=CARTESIAN_POINT('',(1.,0.2675,0.5925));
#9285=CARTESIAN_POINT('Origin',(0.,0.,0.6));
#9286=CARTESIAN_POINT('',(1.,-0.26,0.6));
#9287=CARTESIAN_POINT('',(-0.75,-0.26,0.6));
#9288=CARTESIAN_POINT('',(1.,0.,0.6));
#9289=CARTESIAN_POINT('Origin',(1.,0.,0.35));
#9290=CARTESIAN_POINT('',(1.,-0.26,0.));
#9291=CARTESIAN_POINT('',(1.,-0.3,0.04));
#9292=CARTESIAN_POINT('',(1.,-0.2925,0.0325));
#9293=CARTESIAN_POINT('',(1.,0.,0.));
#9294=CARTESIAN_POINT('',(1.,-0.3,0.56));
#9295=CARTESIAN_POINT('',(1.,-0.2675,0.5925));
#9296=CARTESIAN_POINT('',(1.,-0.3,0.175));
#9297=CARTESIAN_POINT('Origin',(0.,0.,0.));
#9298=CARTESIAN_POINT('',(-0.75,-0.26,0.));
#9299=CARTESIAN_POINT('Origin',(-0.75,-0.28,0.58));
#9300=CARTESIAN_POINT('',(-0.75,-0.3,0.56));
#9301=CARTESIAN_POINT('Origin',(-0.75,-0.28,0.02));
#9302=CARTESIAN_POINT('',(-0.75,-0.3,0.04));
#9303=CARTESIAN_POINT('Origin',(-1.5,-0.3,0.));
#9304=CARTESIAN_POINT('',(0.,0.,0.));
#9305=CARTESIAN_POINT('Origin',(0.375,0.5,0.));
#9306=CARTESIAN_POINT('',(-0.375,0.5,-4.59242549680257E-17));
#9307=CARTESIAN_POINT('Origin',(0.,0.5,0.));
#9308=CARTESIAN_POINT('Origin',(0.,0.475,0.));
#9309=CARTESIAN_POINT('',(-0.425,0.45,-5.20474889637625E-17));
#9310=CARTESIAN_POINT('Origin',(0.,0.45,0.));
#9311=CARTESIAN_POINT('',(-0.4,0.475,-4.89858719658941E-17));
#9312=CARTESIAN_POINT('Origin',(0.,0.24,0.));
#9313=CARTESIAN_POINT('',(-0.425,0.0299999999999998,-5.20474889637625E-17));
#9314=CARTESIAN_POINT('Origin',(0.,0.0299999999999998,0.));
#9315=CARTESIAN_POINT('',(-0.425,0.24,-5.20474889637625E-17));
#9316=CARTESIAN_POINT('Origin',(0.,0.0150000000000001,0.));
#9317=CARTESIAN_POINT('',(-0.395,4.85722573273506E-17,-4.83735485663204E-17));
#9318=CARTESIAN_POINT('Origin',(0.,0.,0.));
#9319=CARTESIAN_POINT('',(-0.41,0.0150000000000001,-5.02105187650415E-17));
#9320=CARTESIAN_POINT('Origin',(0.27,0.,0.));
#9321=CARTESIAN_POINT('',(-0.27,0.,-3.30654635769785E-17));
#9322=CARTESIAN_POINT('Origin',(0.,0.,0.));
#9323=CARTESIAN_POINT('Origin',(0.,-0.02,0.));
#9324=CARTESIAN_POINT('',(-0.24505,-0.0498999999999999,3.00099698131059E-17));
#9325=CARTESIAN_POINT('Origin',(0.,-0.0498999999999999,0.));
#9326=CARTESIAN_POINT('',(-0.26,-0.02,-3.18408167778312E-17));
#9327=CARTESIAN_POINT('Origin',(0.,-0.995,0.));
#9328=CARTESIAN_POINT('',(-0.24505,-1.95495,3.00099698131059E-17));
#9329=CARTESIAN_POINT('Origin',(0.,-1.95495,0.));
#9330=CARTESIAN_POINT('',(-0.24505,-0.995,-3.00099698131059E-17));
#9331=CARTESIAN_POINT('Origin',(0.,-1.975,0.));
#9332=CARTESIAN_POINT('',(-0.2,-2.,-2.44929359829471E-17));
#9333=CARTESIAN_POINT('Origin',(0.,-2.,0.));
#9334=CARTESIAN_POINT('',(-0.225,-1.975,-2.75545529808154E-17));
#9335=CARTESIAN_POINT('Origin',(0.,-2.,0.));
#9336=CARTESIAN_POINT('Origin',(0.115470053837925,-0.5,-0.2));
#9337=CARTESIAN_POINT('',(0.23094010767585,-0.5,0.));
#9338=CARTESIAN_POINT('',(0.115470053837925,-0.5,-0.2));
#9339=CARTESIAN_POINT('',(0.23094010767585,-0.5,0.));
#9340=CARTESIAN_POINT('',(0.115470053837925,-0.8,-0.2));
#9341=CARTESIAN_POINT('',(0.115470053837925,-0.5,-0.2));
#9342=CARTESIAN_POINT('',(0.23094010767585,-0.8,0.));
#9343=CARTESIAN_POINT('',(0.23094010767585,-0.8,0.));
#9344=CARTESIAN_POINT('',(0.23094010767585,-0.5,0.));
#9345=CARTESIAN_POINT('Origin',(-0.115470053837925,-0.5,-0.2));
#9346=CARTESIAN_POINT('',(-0.115470053837925,-0.5,-0.2));
#9347=CARTESIAN_POINT('',(0.115470053837925,-0.5,-0.2));
#9348=CARTESIAN_POINT('',(-0.115470053837925,-0.8,-0.2));
#9349=CARTESIAN_POINT('',(-0.115470053837925,-0.5,-0.2));
#9350=CARTESIAN_POINT('',(0.115470053837925,-0.8,-0.2));
#9351=CARTESIAN_POINT('Origin',(-0.23094010767585,-0.5,-2.77555756156289E-17));
#9352=CARTESIAN_POINT('',(-0.23094010767585,-0.5,-2.82820063659975E-17));
#9353=CARTESIAN_POINT('',(-0.115470053837925,-0.5,-0.2));
#9354=CARTESIAN_POINT('',(-0.23094010767585,-0.8,-2.77555756156289E-17));
#9355=CARTESIAN_POINT('',(-0.23094010767585,-0.5,-2.82820063659975E-17));
#9356=CARTESIAN_POINT('',(-0.115470053837925,-0.8,-0.2));
#9357=CARTESIAN_POINT('Origin',(-0.115470053837925,-0.5,0.2));
#9358=CARTESIAN_POINT('',(-0.115470053837925,-0.5,0.2));
#9359=CARTESIAN_POINT('',(-0.23094010767585,-0.5,-2.82820063659975E-17));
#9360=CARTESIAN_POINT('',(-0.115470053837925,-0.8,0.2));
#9361=CARTESIAN_POINT('',(-0.115470053837925,-0.5,0.2));
#9362=CARTESIAN_POINT('',(-0.23094010767585,-0.8,-2.82820063659975E-17));
#9363=CARTESIAN_POINT('Origin',(0.115470053837925,-0.5,0.2));
#9364=CARTESIAN_POINT('',(0.115470053837925,-0.5,0.2));
#9365=CARTESIAN_POINT('',(-0.115470053837925,-0.5,0.2));
#9366=CARTESIAN_POINT('',(0.115470053837925,-0.8,0.2));
#9367=CARTESIAN_POINT('',(0.115470053837925,-0.5,0.2));
#9368=CARTESIAN_POINT('',(-0.115470053837925,-0.8,0.2));
#9369=CARTESIAN_POINT('Origin',(0.23094010767585,-0.5,0.));
#9370=CARTESIAN_POINT('',(0.115470053837925,-0.5,0.2));
#9371=CARTESIAN_POINT('',(0.115470053837925,-0.8,0.2));
#9372=CARTESIAN_POINT('Origin',(0.,-0.5,0.));
#9373=CARTESIAN_POINT('Origin',(0.,-0.8,0.));
#9374=CARTESIAN_POINT('',(0.,0.,0.));
#9375=CARTESIAN_POINT('',(0.,0.,0.));
#9376=CARTESIAN_POINT('',(0.,0.,0.));
#9377=CARTESIAN_POINT('',(0.,0.,0.));
#9378=CARTESIAN_POINT('',(0.,0.,0.));
#9379=CARTESIAN_POINT('',(0.,-4.5,4.5));
#9380=CARTESIAN_POINT('',(0.,6.8,6.3));
#9381=CARTESIAN_POINT('',(0.,9.,3.85));
#9382=CARTESIAN_POINT('',(0.,10.2,4.5));
#9383=CARTESIAN_POINT('',(0.,0.,0.));
#9384=CARTESIAN_POINT('',(0.,0.,0.));
#9385=UNCERTAINTY_MEASURE_WITH_UNIT(LENGTH_MEASURE(0.001),#9449,
'DISTANCE_ACCURACY_VALUE',
'Maximum model space distance between geometric entities at asserted c
onnectivities');
#9386=UNCERTAINTY_MEASURE_WITH_UNIT(LENGTH_MEASURE(0.001),#9449,
'DISTANCE_ACCURACY_VALUE',
'Maximum model space distance between geometric entities at asserted c
onnectivities');
#9387=UNCERTAINTY_MEASURE_WITH_UNIT(LENGTH_MEASURE(0.001),#9449,
'DISTANCE_ACCURACY_VALUE',
'Maximum model space distance between geometric entities at asserted c
onnectivities');
#9388=UNCERTAINTY_MEASURE_WITH_UNIT(LENGTH_MEASURE(0.001),#9449,
'DISTANCE_ACCURACY_VALUE',
'Maximum model space distance between geometric entities at asserted c
onnectivities');
#9389=UNCERTAINTY_MEASURE_WITH_UNIT(LENGTH_MEASURE(0.001),#9449,
'DISTANCE_ACCURACY_VALUE',
'Maximum model space distance between geometric entities at asserted c
onnectivities');
#9390=UNCERTAINTY_MEASURE_WITH_UNIT(LENGTH_MEASURE(0.001),#9449,
'DISTANCE_ACCURACY_VALUE',
'Maximum model space distance between geometric entities at asserted c
onnectivities');
#9391=UNCERTAINTY_MEASURE_WITH_UNIT(LENGTH_MEASURE(0.001),#9449,
'DISTANCE_ACCURACY_VALUE',
'Maximum model space distance between geometric entities at asserted c
onnectivities');
#9392=UNCERTAINTY_MEASURE_WITH_UNIT(LENGTH_MEASURE(0.001),#9449,
'DISTANCE_ACCURACY_VALUE',
'Maximum model space distance between geometric entities at asserted c
onnectivities');
#9393=UNCERTAINTY_MEASURE_WITH_UNIT(LENGTH_MEASURE(0.001),#9449,
'DISTANCE_ACCURACY_VALUE',
'Maximum model space distance between geometric entities at asserted c
onnectivities');
#9394=UNCERTAINTY_MEASURE_WITH_UNIT(LENGTH_MEASURE(0.001),#9449,
'DISTANCE_ACCURACY_VALUE',
'Maximum model space distance between geometric entities at asserted c
onnectivities');
#9395=UNCERTAINTY_MEASURE_WITH_UNIT(LENGTH_MEASURE(0.001),#9449,
'DISTANCE_ACCURACY_VALUE',
'Maximum model space distance between geometric entities at asserted c
onnectivities');
#9396=UNCERTAINTY_MEASURE_WITH_UNIT(LENGTH_MEASURE(0.001),#9449,
'DISTANCE_ACCURACY_VALUE',
'Maximum model space distance between geometric entities at asserted c
onnectivities');
#9397=UNCERTAINTY_MEASURE_WITH_UNIT(LENGTH_MEASURE(0.001),#9449,
'DISTANCE_ACCURACY_VALUE',
'Maximum model space distance between geometric entities at asserted c
onnectivities');
#9398=UNCERTAINTY_MEASURE_WITH_UNIT(LENGTH_MEASURE(0.001),#9449,
'DISTANCE_ACCURACY_VALUE',
'Maximum model space distance between geometric entities at asserted c
onnectivities');
#9399=UNCERTAINTY_MEASURE_WITH_UNIT(LENGTH_MEASURE(0.001),#9449,
'DISTANCE_ACCURACY_VALUE',
'Maximum model space distance between geometric entities at asserted c
onnectivities');
#9400=UNCERTAINTY_MEASURE_WITH_UNIT(LENGTH_MEASURE(0.001),#9449,
'DISTANCE_ACCURACY_VALUE',
'Maximum model space distance between geometric entities at asserted c
onnectivities');
#9401=UNCERTAINTY_MEASURE_WITH_UNIT(LENGTH_MEASURE(0.001),#9449,
'DISTANCE_ACCURACY_VALUE',
'Maximum model space distance between geometric entities at asserted c
onnectivities');
#9402=UNCERTAINTY_MEASURE_WITH_UNIT(LENGTH_MEASURE(0.001),#9449,
'DISTANCE_ACCURACY_VALUE',
'Maximum model space distance between geometric entities at asserted c
onnectivities');
#9403=UNCERTAINTY_MEASURE_WITH_UNIT(LENGTH_MEASURE(0.001),#9449,
'DISTANCE_ACCURACY_VALUE',
'Maximum model space distance between geometric entities at asserted c
onnectivities');
#9404=UNCERTAINTY_MEASURE_WITH_UNIT(LENGTH_MEASURE(0.001),#9449,
'DISTANCE_ACCURACY_VALUE',
'Maximum model space distance between geometric entities at asserted c
onnectivities');
#9405=UNCERTAINTY_MEASURE_WITH_UNIT(LENGTH_MEASURE(0.001),#9449,
'DISTANCE_ACCURACY_VALUE',
'Maximum model space distance between geometric entities at asserted c
onnectivities');
#9406=UNCERTAINTY_MEASURE_WITH_UNIT(LENGTH_MEASURE(0.001),#9449,
'DISTANCE_ACCURACY_VALUE',
'Maximum model space distance between geometric entities at asserted c
onnectivities');
#9407=UNCERTAINTY_MEASURE_WITH_UNIT(LENGTH_MEASURE(0.001),#9449,
'DISTANCE_ACCURACY_VALUE',
'Maximum model space distance between geometric entities at asserted c
onnectivities');
#9408=UNCERTAINTY_MEASURE_WITH_UNIT(LENGTH_MEASURE(0.001),#9449,
'DISTANCE_ACCURACY_VALUE',
'Maximum model space distance between geometric entities at asserted c
onnectivities');
#9409=UNCERTAINTY_MEASURE_WITH_UNIT(LENGTH_MEASURE(0.001),#9449,
'DISTANCE_ACCURACY_VALUE',
'Maximum model space distance between geometric entities at asserted c
onnectivities');
#9410=UNCERTAINTY_MEASURE_WITH_UNIT(LENGTH_MEASURE(0.001),#9449,
'DISTANCE_ACCURACY_VALUE',
'Maximum model space distance between geometric entities at asserted c
onnectivities');
#9411=UNCERTAINTY_MEASURE_WITH_UNIT(LENGTH_MEASURE(0.001),#9449,
'DISTANCE_ACCURACY_VALUE',
'Maximum model space distance between geometric entities at asserted c
onnectivities');
#9412=UNCERTAINTY_MEASURE_WITH_UNIT(LENGTH_MEASURE(0.001),#9449,
'DISTANCE_ACCURACY_VALUE',
'Maximum model space distance between geometric entities at asserted c
onnectivities');
#9413=UNCERTAINTY_MEASURE_WITH_UNIT(LENGTH_MEASURE(0.001),#9449,
'DISTANCE_ACCURACY_VALUE',
'Maximum model space distance between geometric entities at asserted c
onnectivities');
#9414=UNCERTAINTY_MEASURE_WITH_UNIT(LENGTH_MEASURE(0.001),#9449,
'DISTANCE_ACCURACY_VALUE',
'Maximum model space distance between geometric entities at asserted c
onnectivities');
#9415=UNCERTAINTY_MEASURE_WITH_UNIT(LENGTH_MEASURE(0.001),#9449,
'DISTANCE_ACCURACY_VALUE',
'Maximum model space distance between geometric entities at asserted c
onnectivities');
#9416=UNCERTAINTY_MEASURE_WITH_UNIT(LENGTH_MEASURE(0.001),#9449,
'DISTANCE_ACCURACY_VALUE',
'Maximum model space distance between geometric entities at asserted c
onnectivities');
#9417=(
GEOMETRIC_REPRESENTATION_CONTEXT(3)
GLOBAL_UNCERTAINTY_ASSIGNED_CONTEXT((#9385))
GLOBAL_UNIT_ASSIGNED_CONTEXT((#9449,#9451,#9452))
REPRESENTATION_CONTEXT('','3D')
);
#9418=(
GEOMETRIC_REPRESENTATION_CONTEXT(3)
GLOBAL_UNCERTAINTY_ASSIGNED_CONTEXT((#9386))
GLOBAL_UNIT_ASSIGNED_CONTEXT((#9449,#9451,#9452))
REPRESENTATION_CONTEXT('','3D')
);
#9419=(
GEOMETRIC_REPRESENTATION_CONTEXT(3)
GLOBAL_UNCERTAINTY_ASSIGNED_CONTEXT((#9387))
GLOBAL_UNIT_ASSIGNED_CONTEXT((#9449,#9451,#9452))
REPRESENTATION_CONTEXT('','3D')
);
#9420=(
GEOMETRIC_REPRESENTATION_CONTEXT(3)
GLOBAL_UNCERTAINTY_ASSIGNED_CONTEXT((#9388))
GLOBAL_UNIT_ASSIGNED_CONTEXT((#9449,#9451,#9452))
REPRESENTATION_CONTEXT('','3D')
);
#9421=(
GEOMETRIC_REPRESENTATION_CONTEXT(3)
GLOBAL_UNCERTAINTY_ASSIGNED_CONTEXT((#9389))
GLOBAL_UNIT_ASSIGNED_CONTEXT((#9449,#9451,#9452))
REPRESENTATION_CONTEXT('','3D')
);
#9422=(
GEOMETRIC_REPRESENTATION_CONTEXT(3)
GLOBAL_UNCERTAINTY_ASSIGNED_CONTEXT((#9390))
GLOBAL_UNIT_ASSIGNED_CONTEXT((#9449,#9451,#9452))
REPRESENTATION_CONTEXT('','3D')
);
#9423=(
GEOMETRIC_REPRESENTATION_CONTEXT(3)
GLOBAL_UNCERTAINTY_ASSIGNED_CONTEXT((#9391))
GLOBAL_UNIT_ASSIGNED_CONTEXT((#9449,#9451,#9452))
REPRESENTATION_CONTEXT('','3D')
);
#9424=(
GEOMETRIC_REPRESENTATION_CONTEXT(3)
GLOBAL_UNCERTAINTY_ASSIGNED_CONTEXT((#9392))
GLOBAL_UNIT_ASSIGNED_CONTEXT((#9449,#9451,#9452))
REPRESENTATION_CONTEXT('','3D')
);
#9425=(
GEOMETRIC_REPRESENTATION_CONTEXT(3)
GLOBAL_UNCERTAINTY_ASSIGNED_CONTEXT((#9393))
GLOBAL_UNIT_ASSIGNED_CONTEXT((#9449,#9451,#9452))
REPRESENTATION_CONTEXT('','3D')
);
#9426=(
GEOMETRIC_REPRESENTATION_CONTEXT(3)
GLOBAL_UNCERTAINTY_ASSIGNED_CONTEXT((#9394))
GLOBAL_UNIT_ASSIGNED_CONTEXT((#9449,#9451,#9452))
REPRESENTATION_CONTEXT('','3D')
);
#9427=(
GEOMETRIC_REPRESENTATION_CONTEXT(3)
GLOBAL_UNCERTAINTY_ASSIGNED_CONTEXT((#9395))
GLOBAL_UNIT_ASSIGNED_CONTEXT((#9449,#9451,#9452))
REPRESENTATION_CONTEXT('','3D')
);
#9428=(
GEOMETRIC_REPRESENTATION_CONTEXT(3)
GLOBAL_UNCERTAINTY_ASSIGNED_CONTEXT((#9396))
GLOBAL_UNIT_ASSIGNED_CONTEXT((#9449,#9451,#9452))
REPRESENTATION_CONTEXT('','3D')
);
#9429=(
GEOMETRIC_REPRESENTATION_CONTEXT(3)
GLOBAL_UNCERTAINTY_ASSIGNED_CONTEXT((#9397))
GLOBAL_UNIT_ASSIGNED_CONTEXT((#9449,#9451,#9452))
REPRESENTATION_CONTEXT('','3D')
);
#9430=(
GEOMETRIC_REPRESENTATION_CONTEXT(3)
GLOBAL_UNCERTAINTY_ASSIGNED_CONTEXT((#9398))
GLOBAL_UNIT_ASSIGNED_CONTEXT((#9449,#9451,#9452))
REPRESENTATION_CONTEXT('','3D')
);
#9431=(
GEOMETRIC_REPRESENTATION_CONTEXT(3)
GLOBAL_UNCERTAINTY_ASSIGNED_CONTEXT((#9399))
GLOBAL_UNIT_ASSIGNED_CONTEXT((#9449,#9451,#9452))
REPRESENTATION_CONTEXT('','3D')
);
#9432=(
GEOMETRIC_REPRESENTATION_CONTEXT(3)
GLOBAL_UNCERTAINTY_ASSIGNED_CONTEXT((#9400))
GLOBAL_UNIT_ASSIGNED_CONTEXT((#9449,#9451,#9452))
REPRESENTATION_CONTEXT('','3D')
);
#9433=(
GEOMETRIC_REPRESENTATION_CONTEXT(3)
GLOBAL_UNCERTAINTY_ASSIGNED_CONTEXT((#9401))
GLOBAL_UNIT_ASSIGNED_CONTEXT((#9449,#9451,#9452))
REPRESENTATION_CONTEXT('','3D')
);
#9434=(
GEOMETRIC_REPRESENTATION_CONTEXT(3)
GLOBAL_UNCERTAINTY_ASSIGNED_CONTEXT((#9402))
GLOBAL_UNIT_ASSIGNED_CONTEXT((#9449,#9451,#9452))
REPRESENTATION_CONTEXT('','3D')
);
#9435=(
GEOMETRIC_REPRESENTATION_CONTEXT(3)
GLOBAL_UNCERTAINTY_ASSIGNED_CONTEXT((#9403))
GLOBAL_UNIT_ASSIGNED_CONTEXT((#9449,#9451,#9452))
REPRESENTATION_CONTEXT('','3D')
);
#9436=(
GEOMETRIC_REPRESENTATION_CONTEXT(3)
GLOBAL_UNCERTAINTY_ASSIGNED_CONTEXT((#9404))
GLOBAL_UNIT_ASSIGNED_CONTEXT((#9449,#9451,#9452))
REPRESENTATION_CONTEXT('','3D')
);
#9437=(
GEOMETRIC_REPRESENTATION_CONTEXT(3)
GLOBAL_UNCERTAINTY_ASSIGNED_CONTEXT((#9405))
GLOBAL_UNIT_ASSIGNED_CONTEXT((#9449,#9451,#9452))
REPRESENTATION_CONTEXT('','3D')
);
#9438=(
GEOMETRIC_REPRESENTATION_CONTEXT(3)
GLOBAL_UNCERTAINTY_ASSIGNED_CONTEXT((#9406))
GLOBAL_UNIT_ASSIGNED_CONTEXT((#9449,#9451,#9452))
REPRESENTATION_CONTEXT('','3D')
);
#9439=(
GEOMETRIC_REPRESENTATION_CONTEXT(3)
GLOBAL_UNCERTAINTY_ASSIGNED_CONTEXT((#9407))
GLOBAL_UNIT_ASSIGNED_CONTEXT((#9449,#9451,#9452))
REPRESENTATION_CONTEXT('','3D')
);
#9440=(
GEOMETRIC_REPRESENTATION_CONTEXT(3)
GLOBAL_UNCERTAINTY_ASSIGNED_CONTEXT((#9408))
GLOBAL_UNIT_ASSIGNED_CONTEXT((#9449,#9451,#9452))
REPRESENTATION_CONTEXT('','3D')
);
#9441=(
GEOMETRIC_REPRESENTATION_CONTEXT(3)
GLOBAL_UNCERTAINTY_ASSIGNED_CONTEXT((#9409))
GLOBAL_UNIT_ASSIGNED_CONTEXT((#9449,#9451,#9452))
REPRESENTATION_CONTEXT('','3D')
);
#9442=(
GEOMETRIC_REPRESENTATION_CONTEXT(3)
GLOBAL_UNCERTAINTY_ASSIGNED_CONTEXT((#9410))
GLOBAL_UNIT_ASSIGNED_CONTEXT((#9449,#9451,#9452))
REPRESENTATION_CONTEXT('','3D')
);
#9443=(
GEOMETRIC_REPRESENTATION_CONTEXT(3)
GLOBAL_UNCERTAINTY_ASSIGNED_CONTEXT((#9411))
GLOBAL_UNIT_ASSIGNED_CONTEXT((#9449,#9451,#9452))
REPRESENTATION_CONTEXT('','3D')
);
#9444=(
GEOMETRIC_REPRESENTATION_CONTEXT(3)
GLOBAL_UNCERTAINTY_ASSIGNED_CONTEXT((#9412))
GLOBAL_UNIT_ASSIGNED_CONTEXT((#9449,#9451,#9452))
REPRESENTATION_CONTEXT('','3D')
);
#9445=(
GEOMETRIC_REPRESENTATION_CONTEXT(3)
GLOBAL_UNCERTAINTY_ASSIGNED_CONTEXT((#9413))
GLOBAL_UNIT_ASSIGNED_CONTEXT((#9449,#9451,#9452))
REPRESENTATION_CONTEXT('','3D')
);
#9446=(
GEOMETRIC_REPRESENTATION_CONTEXT(3)
GLOBAL_UNCERTAINTY_ASSIGNED_CONTEXT((#9414))
GLOBAL_UNIT_ASSIGNED_CONTEXT((#9449,#9451,#9452))
REPRESENTATION_CONTEXT('','3D')
);
#9447=(
GEOMETRIC_REPRESENTATION_CONTEXT(3)
GLOBAL_UNCERTAINTY_ASSIGNED_CONTEXT((#9415))
GLOBAL_UNIT_ASSIGNED_CONTEXT((#9449,#9451,#9452))
REPRESENTATION_CONTEXT('','3D')
);
#9448=(
GEOMETRIC_REPRESENTATION_CONTEXT(3)
GLOBAL_UNCERTAINTY_ASSIGNED_CONTEXT((#9416))
GLOBAL_UNIT_ASSIGNED_CONTEXT((#9449,#9451,#9452))
REPRESENTATION_CONTEXT('','3D')
);
#9449=(
LENGTH_UNIT()
NAMED_UNIT(*)
SI_UNIT(.CENTI.,.METRE.)
);
#9450=(
LENGTH_UNIT()
NAMED_UNIT(*)
SI_UNIT($,.METRE.)
);
#9451=(
NAMED_UNIT(*)
PLANE_ANGLE_UNIT()
SI_UNIT($,.RADIAN.)
);
#9452=(
NAMED_UNIT(*)
SI_UNIT($,.STERADIAN.)
SOLID_ANGLE_UNIT()
);
#9453=SHAPE_DEFINITION_REPRESENTATION(#9484,#9557);
#9454=SHAPE_DEFINITION_REPRESENTATION(#9485,#9558);
#9455=SHAPE_DEFINITION_REPRESENTATION(#9486,#9559);
#9456=SHAPE_DEFINITION_REPRESENTATION(#9487,#9560);
#9457=SHAPE_DEFINITION_REPRESENTATION(#9488,#9561);
#9458=SHAPE_DEFINITION_REPRESENTATION(#9489,#9562);
#9459=SHAPE_DEFINITION_REPRESENTATION(#9490,#9563);
#9460=SHAPE_DEFINITION_REPRESENTATION(#9491,#9564);
#9461=SHAPE_DEFINITION_REPRESENTATION(#9492,#9565);
#9462=SHAPE_DEFINITION_REPRESENTATION(#9493,#9566);
#9463=SHAPE_DEFINITION_REPRESENTATION(#9494,#9567);
#9464=SHAPE_DEFINITION_REPRESENTATION(#9495,#9568);
#9465=SHAPE_DEFINITION_REPRESENTATION(#9496,#9569);
#9466=SHAPE_DEFINITION_REPRESENTATION(#9497,#9570);
#9467=SHAPE_DEFINITION_REPRESENTATION(#9498,#9571);
#9468=SHAPE_DEFINITION_REPRESENTATION(#9499,#9572);
#9469=SHAPE_DEFINITION_REPRESENTATION(#9500,#9573);
#9470=SHAPE_DEFINITION_REPRESENTATION(#9501,#9574);
#9471=SHAPE_DEFINITION_REPRESENTATION(#9502,#9575);
#9472=SHAPE_DEFINITION_REPRESENTATION(#9508,#9576);
#9473=SHAPE_DEFINITION_REPRESENTATION(#9509,#9577);
#9474=SHAPE_DEFINITION_REPRESENTATION(#9510,#9578);
#9475=SHAPE_DEFINITION_REPRESENTATION(#9511,#9579);
#9476=SHAPE_DEFINITION_REPRESENTATION(#9512,#9580);
#9477=SHAPE_DEFINITION_REPRESENTATION(#9513,#9581);
#9478=SHAPE_DEFINITION_REPRESENTATION(#9514,#9582);
#9479=SHAPE_DEFINITION_REPRESENTATION(#9515,#9583);
#9480=SHAPE_DEFINITION_REPRESENTATION(#9516,#9584);
#9481=SHAPE_DEFINITION_REPRESENTATION(#9543,#9585);
#9482=SHAPE_DEFINITION_REPRESENTATION(#9544,#9586);
#9483=SHAPE_DEFINITION_REPRESENTATION(#9545,#9587);
#9484=PRODUCT_DEFINITION_SHAPE('',$,#9589);
#9485=PRODUCT_DEFINITION_SHAPE('',$,#9590);
#9486=PRODUCT_DEFINITION_SHAPE('',$,#9591);
#9487=PRODUCT_DEFINITION_SHAPE('',$,#9592);
#9488=PRODUCT_DEFINITION_SHAPE('',$,#9593);
#9489=PRODUCT_DEFINITION_SHAPE('',$,#9594);
#9490=PRODUCT_DEFINITION_SHAPE('',$,#9595);
#9491=PRODUCT_DEFINITION_SHAPE('',$,#9596);
#9492=PRODUCT_DEFINITION_SHAPE('',$,#9597);
#9493=PRODUCT_DEFINITION_SHAPE('',$,#9598);
#9494=PRODUCT_DEFINITION_SHAPE('',$,#9599);
#9495=PRODUCT_DEFINITION_SHAPE('',$,#9600);
#9496=PRODUCT_DEFINITION_SHAPE('',$,#9601);
#9497=PRODUCT_DEFINITION_SHAPE('',$,#9602);
#9498=PRODUCT_DEFINITION_SHAPE('',$,#9603);
#9499=PRODUCT_DEFINITION_SHAPE('',$,#9604);
#9500=PRODUCT_DEFINITION_SHAPE('',$,#9605);
#9501=PRODUCT_DEFINITION_SHAPE('',$,#9606);
#9502=PRODUCT_DEFINITION_SHAPE('',$,#9607);
#9503=PRODUCT_DEFINITION_SHAPE($,$,#143);
#9504=PRODUCT_DEFINITION_SHAPE($,$,#144);
#9505=PRODUCT_DEFINITION_SHAPE($,$,#145);
#9506=PRODUCT_DEFINITION_SHAPE($,$,#146);
#9507=PRODUCT_DEFINITION_SHAPE($,$,#147);
#9508=PRODUCT_DEFINITION_SHAPE('',$,#9608);
#9509=PRODUCT_DEFINITION_SHAPE('',$,#9609);
#9510=PRODUCT_DEFINITION_SHAPE('',$,#9610);
#9511=PRODUCT_DEFINITION_SHAPE('',$,#9611);
#9512=PRODUCT_DEFINITION_SHAPE('',$,#9612);
#9513=PRODUCT_DEFINITION_SHAPE('',$,#9613);
#9514=PRODUCT_DEFINITION_SHAPE('',$,#9614);
#9515=PRODUCT_DEFINITION_SHAPE('',$,#9615);
#9516=PRODUCT_DEFINITION_SHAPE('',$,#9616);
#9517=PRODUCT_DEFINITION_SHAPE($,$,#148);
#9518=PRODUCT_DEFINITION_SHAPE($,$,#149);
#9519=PRODUCT_DEFINITION_SHAPE($,$,#150);
#9520=PRODUCT_DEFINITION_SHAPE($,$,#151);
#9521=PRODUCT_DEFINITION_SHAPE($,$,#152);
#9522=PRODUCT_DEFINITION_SHAPE($,$,#153);
#9523=PRODUCT_DEFINITION_SHAPE($,$,#154);
#9524=PRODUCT_DEFINITION_SHAPE($,$,#155);
#9525=PRODUCT_DEFINITION_SHAPE($,$,#156);
#9526=PRODUCT_DEFINITION_SHAPE($,$,#157);
#9527=PRODUCT_DEFINITION_SHAPE($,$,#158);
#9528=PRODUCT_DEFINITION_SHAPE($,$,#159);
#9529=PRODUCT_DEFINITION_SHAPE($,$,#160);
#9530=PRODUCT_DEFINITION_SHAPE($,$,#161);
#9531=PRODUCT_DEFINITION_SHAPE($,$,#162);
#9532=PRODUCT_DEFINITION_SHAPE($,$,#163);
#9533=PRODUCT_DEFINITION_SHAPE($,$,#164);
#9534=PRODUCT_DEFINITION_SHAPE($,$,#165);
#9535=PRODUCT_DEFINITION_SHAPE($,$,#166);
#9536=PRODUCT_DEFINITION_SHAPE($,$,#167);
#9537=PRODUCT_DEFINITION_SHAPE($,$,#168);
#9538=PRODUCT_DEFINITION_SHAPE($,$,#169);
#9539=PRODUCT_DEFINITION_SHAPE($,$,#170);
#9540=PRODUCT_DEFINITION_SHAPE($,$,#171);
#9541=PRODUCT_DEFINITION_SHAPE($,$,#172);
#9542=PRODUCT_DEFINITION_SHAPE($,$,#173);
#9543=PRODUCT_DEFINITION_SHAPE('',$,#9617);
#9544=PRODUCT_DEFINITION_SHAPE('',$,#9618);
#9545=PRODUCT_DEFINITION_SHAPE('',$,#9619);
#9546=PRODUCT_DEFINITION_SHAPE($,$,#174);
#9547=PRODUCT_DEFINITION_SHAPE($,$,#175);
#9548=PRODUCT_DEFINITION_SHAPE($,$,#176);
#9549=PRODUCT_DEFINITION_SHAPE($,$,#177);
#9550=PRODUCT_DEFINITION_SHAPE($,$,#178);
#9551=PRODUCT_DEFINITION_SHAPE($,$,#179);
#9552=PRODUCT_DEFINITION_SHAPE($,$,#180);
#9553=PRODUCT_DEFINITION_SHAPE($,$,#181);
#9554=PRODUCT_DEFINITION_SHAPE($,$,#182);
#9555=PRODUCT_DEFINITION_SHAPE($,$,#183);
#9556=PRODUCT_DEFINITION_SHAPE($,$,#184);
#9557=SHAPE_REPRESENTATION('',(#5204,#5826,#5827),#9417);
#9558=SHAPE_REPRESENTATION('',(#5205,#5737,#5738,#5739,#5740,#5741,#5742,
#5743,#5744,#5745,#5746,#5747,#5748,#5749,#5750,#5751,#5752,#5753,#5754,
#5755,#5756,#5757,#5758,#5759,#5760,#5761,#5762),#9418);
#9559=SHAPE_REPRESENTATION('',(#5206),#9419);
#9560=SHAPE_REPRESENTATION('',(#5225),#9420);
#9561=SHAPE_REPRESENTATION('',(#5305),#9421);
#9562=SHAPE_REPRESENTATION('',(#5322),#9422);
#9563=SHAPE_REPRESENTATION('',(#5326),#9423);
#9564=SHAPE_REPRESENTATION('',(#5343),#9424);
#9565=SHAPE_REPRESENTATION('',(#5347),#9425);
#9566=SHAPE_REPRESENTATION('',(#5363),#9426);
#9567=SHAPE_REPRESENTATION('',(#5388),#9427);
#9568=SHAPE_REPRESENTATION('',(#5413),#9428);
#9569=SHAPE_REPRESENTATION('',(#5420),#9429);
#9570=SHAPE_REPRESENTATION('',(#5427,#5556,#5557,#5558,#5559,#5560),#9430);
#9571=SHAPE_REPRESENTATION('',(#5428),#9431);
#9572=SHAPE_REPRESENTATION('',(#5448),#9432);
#9573=SHAPE_REPRESENTATION('',(#5468),#9433);
#9574=SHAPE_REPRESENTATION('',(#5485),#9434);
#9575=SHAPE_REPRESENTATION('',(#5539),#9435);
#9576=SHAPE_REPRESENTATION('',(#5561),#9436);
#9577=SHAPE_REPRESENTATION('',(#5587),#9437);
#9578=SHAPE_REPRESENTATION('',(#5613,#5817,#5818,#5819,#5820,#5821,#5822,
#5823,#5824,#5825),#9438);
#9579=SHAPE_REPRESENTATION('',(#5614),#9439);
#9580=SHAPE_REPRESENTATION('',(#5652),#9440);
#9581=SHAPE_REPRESENTATION('',(#5661),#9441);
#9582=SHAPE_REPRESENTATION('',(#5676),#9442);
#9583=SHAPE_REPRESENTATION('',(#5704),#9443);
#9584=SHAPE_REPRESENTATION('',(#5713),#9444);
#9585=SHAPE_REPRESENTATION('',(#5763),#9445);
#9586=SHAPE_REPRESENTATION('',(#5780),#9446);
#9587=SHAPE_REPRESENTATION('',(#5791),#9447);
#9588=PRODUCT_DEFINITION_CONTEXT('part definition',#9683,'design');
#9589=PRODUCT_DEFINITION('PAT-089','PAT-089',#9620,
#9588);
#9590=PRODUCT_DEFINITION('Housing and glands','Housing and glands',#9621,
#9588);
#9591=PRODUCT_DEFINITION('Base','Base',#9622,#9588);
#9592=PRODUCT_DEFINITION('Housing','Housing',#9623,#9588);
#9593=PRODUCT_DEFINITION('Seal gland','Seal gland',#9624,#9588);
#9594=PRODUCT_DEFINITION('Shaft seal','Shaft seal',#9625,#9588);
#9595=PRODUCT_DEFINITION('Seal gland (1)','Seal gland (1)',#9626,#9588);
#9596=PRODUCT_DEFINITION('Shaft seal (1)','Shaft seal (1)',#9627,#9588);
#9597=PRODUCT_DEFINITION('Distribution sleeve','Distribution sleeve',#9628,
#9588);
#9598=PRODUCT_DEFINITION('Bearing cap','Bearing cap',#9629,#9588);
#9599=PRODUCT_DEFINITION('Bearing cap (1)','Bearing cap (1)',#9630,#9588);
#9600=PRODUCT_DEFINITION('Bonded foot pad','Bonded foot pad',#9631,#9588);
#9601=PRODUCT_DEFINITION('Bonded foot pad (1)','Bonded foot pad (1)',#9632,
#9588);
#9602=PRODUCT_DEFINITION('Sealed Ball Bearing - 20 x 47 x 14 mm',
'Sealed Ball Bearing - 20 x 47 x 14 mm',#9633,#9588);
#9603=PRODUCT_DEFINITION('Inner ring','Inner ring',#9634,#9588);
#9604=PRODUCT_DEFINITION('Outer ring','Outer ring',#9635,#9588);
#9605=PRODUCT_DEFINITION('Balls','Balls',#9636,#9588);
#9606=PRODUCT_DEFINITION('Cage','Cage',#9637,#9588);
#9607=PRODUCT_DEFINITION('Seals 2RS','Seals 2RS',#9638,#9588);
#9608=PRODUCT_DEFINITION('Cap Screw - M6x25','Cap Screw - M6x25',#9639,
#9588);
#9609=PRODUCT_DEFINITION('Cap Screw - M4x16','Cap Screw - M4x16',#9640,
#9588);
#9610=PRODUCT_DEFINITION('Hollow shaft and drive',
'Hollow shaft and drive',#9641,#9588);
#9611=PRODUCT_DEFINITION('Hollow spindle','Hollow spindle',#9642,#9588);
#9612=PRODUCT_DEFINITION('Inner race spacer','Inner race spacer',#9643,
#9588);
#9613=PRODUCT_DEFINITION('Shaft collar','Shaft collar',#9644,#9588);
#9614=PRODUCT_DEFINITION('Drive flange','Drive flange',#9645,#9588);
#9615=PRODUCT_DEFINITION('End keeper','End keeper',#9646,#9588);
#9616=PRODUCT_DEFINITION(
'Hex Pipe Nipple - 1-4 Inch Tapered Pipe Thread',
'Hex Pipe Nipple - 1-4 Inch Tapered Pipe Thread',#9647,#9588);
#9617=PRODUCT_DEFINITION('Socket Set Screw - M5x8',
'Socket Set Screw - M5x8',#9648,#9588);
#9618=PRODUCT_DEFINITION('Key 6x6x20','Key 6x6x20',#9649,#9588);
#9619=PRODUCT_DEFINITION('Cap Screw - M5x20','Cap Screw - M5x20',#9650,
#9588);
#9620=PRODUCT_DEFINITION_FORMATION('',$,#9685);
#9621=PRODUCT_DEFINITION_FORMATION('',$,#9686);
#9622=PRODUCT_DEFINITION_FORMATION('',$,#9687);
#9623=PRODUCT_DEFINITION_FORMATION('',$,#9688);
#9624=PRODUCT_DEFINITION_FORMATION('',$,#9689);
#9625=PRODUCT_DEFINITION_FORMATION('',$,#9690);
#9626=PRODUCT_DEFINITION_FORMATION('',$,#9691);
#9627=PRODUCT_DEFINITION_FORMATION('',$,#9692);
#9628=PRODUCT_DEFINITION_FORMATION('',$,#9693);
#9629=PRODUCT_DEFINITION_FORMATION('',$,#9694);
#9630=PRODUCT_DEFINITION_FORMATION('',$,#9695);
#9631=PRODUCT_DEFINITION_FORMATION('',$,#9696);
#9632=PRODUCT_DEFINITION_FORMATION('',$,#9697);
#9633=PRODUCT_DEFINITION_FORMATION('',$,#9698);
#9634=PRODUCT_DEFINITION_FORMATION('',$,#9699);
#9635=PRODUCT_DEFINITION_FORMATION('',$,#9700);
#9636=PRODUCT_DEFINITION_FORMATION('',$,#9701);
#9637=PRODUCT_DEFINITION_FORMATION('',$,#9702);
#9638=PRODUCT_DEFINITION_FORMATION('',$,#9703);
#9639=PRODUCT_DEFINITION_FORMATION('',$,#9704);
#9640=PRODUCT_DEFINITION_FORMATION('',$,#9705);
#9641=PRODUCT_DEFINITION_FORMATION('',$,#9706);
#9642=PRODUCT_DEFINITION_FORMATION('',$,#9707);
#9643=PRODUCT_DEFINITION_FORMATION('',$,#9708);
#9644=PRODUCT_DEFINITION_FORMATION('',$,#9709);
#9645=PRODUCT_DEFINITION_FORMATION('',$,#9710);
#9646=PRODUCT_DEFINITION_FORMATION('',$,#9711);
#9647=PRODUCT_DEFINITION_FORMATION('',$,#9712);
#9648=PRODUCT_DEFINITION_FORMATION('',$,#9713);
#9649=PRODUCT_DEFINITION_FORMATION('',$,#9714);
#9650=PRODUCT_DEFINITION_FORMATION('',$,#9715);
#9651=PRODUCT_RELATED_PRODUCT_CATEGORY('PAT-089','PAT-089',(#9685));
#9652=PRODUCT_RELATED_PRODUCT_CATEGORY('Housing and glands',
'Housing and glands',(#9686));
#9653=PRODUCT_RELATED_PRODUCT_CATEGORY('Base','Base',(#9687));
#9654=PRODUCT_RELATED_PRODUCT_CATEGORY('Housing','Housing',(#9688));
#9655=PRODUCT_RELATED_PRODUCT_CATEGORY('Seal gland','Seal gland',(#9689));
#9656=PRODUCT_RELATED_PRODUCT_CATEGORY('Shaft seal','Shaft seal',(#9690));
#9657=PRODUCT_RELATED_PRODUCT_CATEGORY('Seal gland (1)',
'Seal gland (1)',(#9691));
#9658=PRODUCT_RELATED_PRODUCT_CATEGORY('Shaft seal (1)',
'Shaft seal (1)',(#9692));
#9659=PRODUCT_RELATED_PRODUCT_CATEGORY('Distribution sleeve',
'Distribution sleeve',(#9693));
#9660=PRODUCT_RELATED_PRODUCT_CATEGORY('Bearing cap','Bearing cap',(#9694));
#9661=PRODUCT_RELATED_PRODUCT_CATEGORY('Bearing cap (1)',
'Bearing cap (1)',(#9695));
#9662=PRODUCT_RELATED_PRODUCT_CATEGORY('Bonded foot pad',
'Bonded foot pad',(#9696));
#9663=PRODUCT_RELATED_PRODUCT_CATEGORY('Bonded foot pad (1)',
'Bonded foot pad (1)',(#9697));
#9664=PRODUCT_RELATED_PRODUCT_CATEGORY(
'Sealed Ball Bearing - 20 x 47 x 14 mm',
'Sealed Ball Bearing - 20 x 47 x 14 mm',(#9698));
#9665=PRODUCT_RELATED_PRODUCT_CATEGORY('Inner ring','Inner ring',(#9699));
#9666=PRODUCT_RELATED_PRODUCT_CATEGORY('Outer ring','Outer ring',(#9700));
#9667=PRODUCT_RELATED_PRODUCT_CATEGORY('Balls','Balls',(#9701));
#9668=PRODUCT_RELATED_PRODUCT_CATEGORY('Cage','Cage',(#9702));
#9669=PRODUCT_RELATED_PRODUCT_CATEGORY('Seals 2RS','Seals 2RS',(#9703));
#9670=PRODUCT_RELATED_PRODUCT_CATEGORY('Cap Screw - M6x25',
'Cap Screw - M6x25',(#9704));
#9671=PRODUCT_RELATED_PRODUCT_CATEGORY('Cap Screw - M4x16',
'Cap Screw - M4x16',(#9705));
#9672=PRODUCT_RELATED_PRODUCT_CATEGORY('Hollow shaft and drive',
'Hollow shaft and drive',(#9706));
#9673=PRODUCT_RELATED_PRODUCT_CATEGORY('Hollow spindle',
'Hollow spindle',(#9707));
#9674=PRODUCT_RELATED_PRODUCT_CATEGORY('Inner race spacer',
'Inner race spacer',(#9708));
#9675=PRODUCT_RELATED_PRODUCT_CATEGORY('Shaft collar','Shaft collar',(#9709));
#9676=PRODUCT_RELATED_PRODUCT_CATEGORY('Drive flange','Drive flange',(#9710));
#9677=PRODUCT_RELATED_PRODUCT_CATEGORY('End keeper','End keeper',(#9711));
#9678=PRODUCT_RELATED_PRODUCT_CATEGORY(
'Hex Pipe Nipple - 1-4 Inch Tapered Pipe Thread',
'Hex Pipe Nipple - 1-4 Inch Tapered Pipe Thread',(#9712));
#9679=PRODUCT_RELATED_PRODUCT_CATEGORY('Socket Set Screw - M5x8',
'Socket Set Screw - M5x8',(#9713));
#9680=PRODUCT_RELATED_PRODUCT_CATEGORY('Key 6x6x20','Key 6x6x20',(#9714));
#9681=PRODUCT_RELATED_PRODUCT_CATEGORY('Cap Screw - M5x20',
'Cap Screw - M5x20',(#9715));
#9682=APPLICATION_PROTOCOL_DEFINITION('international standard',
'automotive_design',2009,#9683);
#9683=APPLICATION_CONTEXT(
'Core Data for Automotive Mechanical Design Process');
#9684=PRODUCT_CONTEXT('part definition',#9683,'mechanical');
#9685=PRODUCT('PAT-089','PAT-089',
'PAT-089',(#9684));
#9686=PRODUCT('Housing and glands','Housing and glands',
'Housing and glands',(#9684));
#9687=PRODUCT('Base','Base','Base',(#9684));
#9688=PRODUCT('Housing','Housing','Housing',(#9684));
#9689=PRODUCT('Seal gland','Seal gland','Seal gland',(#9684));
#9690=PRODUCT('Shaft seal','Shaft seal','Shaft seal',(#9684));
#9691=PRODUCT('Seal gland (1)','Seal gland (1)','Seal gland (1)',(#9684));
#9692=PRODUCT('Shaft seal (1)','Shaft seal (1)','Shaft seal (1)',(#9684));
#9693=PRODUCT('Distribution sleeve','Distribution sleeve',
'Distribution sleeve',(#9684));
#9694=PRODUCT('Bearing cap','Bearing cap','Bearing cap',(#9684));
#9695=PRODUCT('Bearing cap (1)','Bearing cap (1)','Bearing cap (1)',(#9684));
#9696=PRODUCT('Bonded foot pad','Bonded foot pad','Bonded foot pad',(#9684));
#9697=PRODUCT('Bonded foot pad (1)','Bonded foot pad (1)',
'Bonded foot pad (1)',(#9684));
#9698=PRODUCT('Sealed Ball Bearing - 20 x 47 x 14 mm',
'Sealed Ball Bearing - 20 x 47 x 14 mm',
'Sealed Ball Bearing - 20 x 47 x 14 mm',(#9684));
#9699=PRODUCT('Inner ring','Inner ring','Inner ring',(#9684));
#9700=PRODUCT('Outer ring','Outer ring','Outer ring',(#9684));
#9701=PRODUCT('Balls','Balls','Balls',(#9684));
#9702=PRODUCT('Cage','Cage','Cage',(#9684));
#9703=PRODUCT('Seals 2RS','Seals 2RS','Seals 2RS',(#9684));
#9704=PRODUCT('Cap Screw - M6x25','Cap Screw - M6x25',
'Cap Screw - M6x25',(#9684));
#9705=PRODUCT('Cap Screw - M4x16','Cap Screw - M4x16',
'Cap Screw - M4x16',(#9684));
#9706=PRODUCT('Hollow shaft and drive','Hollow shaft and drive',
'Hollow shaft and drive',(#9684));
#9707=PRODUCT('Hollow spindle','Hollow spindle','Hollow spindle',(#9684));
#9708=PRODUCT('Inner race spacer','Inner race spacer',
'Inner race spacer',(#9684));
#9709=PRODUCT('Shaft collar','Shaft collar','Shaft collar',(#9684));
#9710=PRODUCT('Drive flange','Drive flange','Drive flange',(#9684));
#9711=PRODUCT('End keeper','End keeper','End keeper',(#9684));
#9712=PRODUCT('Hex Pipe Nipple - 1-4 Inch Tapered Pipe Thread',
'Hex Pipe Nipple - 1-4 Inch Tapered Pipe Thread',
'Hex Pipe Nipple - 1-4 Inch Tapered Pipe Thread',(#9684));
#9713=PRODUCT('Socket Set Screw - M5x8','Socket Set Screw - M5x8',
'Socket Set Screw - M5x8',(#9684));
#9714=PRODUCT('Key 6x6x20','Key 6x6x20','Key 6x6x20',(#9684));
#9715=PRODUCT('Cap Screw - M5x20','Cap Screw - M5x20',
'Cap Screw - M5x20',(#9684));
#9716=PRESENTATION_STYLE_ASSIGNMENT((#9721));
#9717=PRESENTATION_STYLE_ASSIGNMENT((#9722));
#9718=PRESENTATION_STYLE_ASSIGNMENT((#9723));
#9719=PRESENTATION_STYLE_ASSIGNMENT((#9724));
#9720=PRESENTATION_STYLE_ASSIGNMENT((#9725));
#9721=SURFACE_STYLE_USAGE(.BOTH.,#9726);
#9722=SURFACE_STYLE_USAGE(.BOTH.,#9727);
#9723=SURFACE_STYLE_USAGE(.BOTH.,#9728);
#9724=SURFACE_STYLE_USAGE(.BOTH.,#9729);
#9725=SURFACE_STYLE_USAGE(.BOTH.,#9730);
#9726=SURFACE_SIDE_STYLE('',(#9731));
#9727=SURFACE_SIDE_STYLE('',(#9732));
#9728=SURFACE_SIDE_STYLE('',(#9733));
#9729=SURFACE_SIDE_STYLE('',(#9734));
#9730=SURFACE_SIDE_STYLE('',(#9735));
#9731=SURFACE_STYLE_FILL_AREA(#9736);
#9732=SURFACE_STYLE_FILL_AREA(#9737);
#9733=SURFACE_STYLE_FILL_AREA(#9738);
#9734=SURFACE_STYLE_FILL_AREA(#9739);
#9735=SURFACE_STYLE_FILL_AREA(#9740);
#9736=FILL_AREA_STYLE('Steel - Satin',(#9741));
#9737=FILL_AREA_STYLE('CAD Library Painted - Deep blue',(#9742));
#9738=FILL_AREA_STYLE('CAD Library Painted - Engineering blue',(#9743));
#9739=FILL_AREA_STYLE('CAD Library Painted - Steel gray',(#9744));
#9740=FILL_AREA_STYLE('CAD Library Painted - Graphite',(#9745));
#9741=FILL_AREA_STYLE_COLOUR('Steel - Satin',#9746);
#9742=FILL_AREA_STYLE_COLOUR('CAD Library Painted - Deep blue',#9747);
#9743=FILL_AREA_STYLE_COLOUR('CAD Library Painted - Engineering blue',#9748);
#9744=FILL_AREA_STYLE_COLOUR('CAD Library Painted - Steel gray',#9749);
#9745=FILL_AREA_STYLE_COLOUR('CAD Library Painted - Graphite',#9750);
#9746=COLOUR_RGB('Steel - Satin',0.627450980392157,0.627450980392157,0.627450980392157);
#9747=COLOUR_RGB('CAD Library Painted - Deep blue',0.0784313725490196,0.203921568627451,
0.349019607843137);
#9748=COLOUR_RGB('CAD Library Painted - Engineering blue',0.12156862745098,
0.356862745098039,0.6);
#9749=COLOUR_RGB('CAD Library Painted - Steel gray',0.592156862745098,0.631372549019608,
0.67843137254902);
#9750=COLOUR_RGB('CAD Library Painted - Graphite',0.168627450980392,0.192156862745098,
0.231372549019608);
#9751=COLOUR_RGB('Dark Blue',0.08,0.2,0.34);
#9752=FILL_AREA_STYLE_COLOUR('',#9751);
#9753=FILL_AREA_STYLE('',(#9752));
#9754=SURFACE_STYLE_FILL_AREA(#9753);
#9755=SURFACE_SIDE_STYLE('',(#9754));
#9756=SURFACE_STYLE_USAGE(.BOTH.,#9755);
#9757=PRESENTATION_STYLE_ASSIGNMENT((#9756));
#9758=COLOUR_RGB('Light Blue',0.38,0.62,0.78);
#9759=FILL_AREA_STYLE_COLOUR('',#9758);
#9760=FILL_AREA_STYLE('',(#9759));
#9761=SURFACE_STYLE_FILL_AREA(#9760);
#9762=SURFACE_SIDE_STYLE('',(#9761));
#9763=SURFACE_STYLE_USAGE(.BOTH.,#9762);
#9764=PRESENTATION_STYLE_ASSIGNMENT((#9763));
#9765=COLOUR_RGB('Sky Blue',0.24,0.69,0.87);
#9766=FILL_AREA_STYLE_COLOUR('',#9765);
#9767=FILL_AREA_STYLE('',(#9766));
#9768=SURFACE_STYLE_FILL_AREA(#9767);
#9769=SURFACE_SIDE_STYLE('',(#9768));
#9770=SURFACE_STYLE_USAGE(.BOTH.,#9769);
#9771=PRESENTATION_STYLE_ASSIGNMENT((#9770));
#9772=COLOUR_RGB('Grey',0.48,0.52,0.57);
#9773=FILL_AREA_STYLE_COLOUR('',#9772);
#9774=FILL_AREA_STYLE('',(#9773));
#9775=SURFACE_STYLE_FILL_AREA(#9774);
#9776=SURFACE_SIDE_STYLE('',(#9775));
#9777=SURFACE_STYLE_USAGE(.BOTH.,#9776);
#9778=PRESENTATION_STYLE_ASSIGNMENT((#9777));
#9779=COLOUR_RGB('Black',0.12,0.14,0.17);
#9780=FILL_AREA_STYLE_COLOUR('',#9779);
#9781=FILL_AREA_STYLE('',(#9780));
#9782=SURFACE_STYLE_FILL_AREA(#9781);
#9783=SURFACE_SIDE_STYLE('',(#9782));
#9784=SURFACE_STYLE_USAGE(.BOTH.,#9783);
#9785=PRESENTATION_STYLE_ASSIGNMENT((#9784));
#9786=COLOUR_RGB('Off White',0.89,0.88,0.83);
#9787=FILL_AREA_STYLE_COLOUR('',#9786);
#9788=FILL_AREA_STYLE('',(#9787));
#9789=SURFACE_STYLE_FILL_AREA(#9788);
#9790=SURFACE_SIDE_STYLE('',(#9789));
#9791=SURFACE_STYLE_USAGE(.BOTH.,#9790);
#9792=PRESENTATION_STYLE_ASSIGNMENT((#9791));
ENDSEC;
END-ISO-10303-21;
